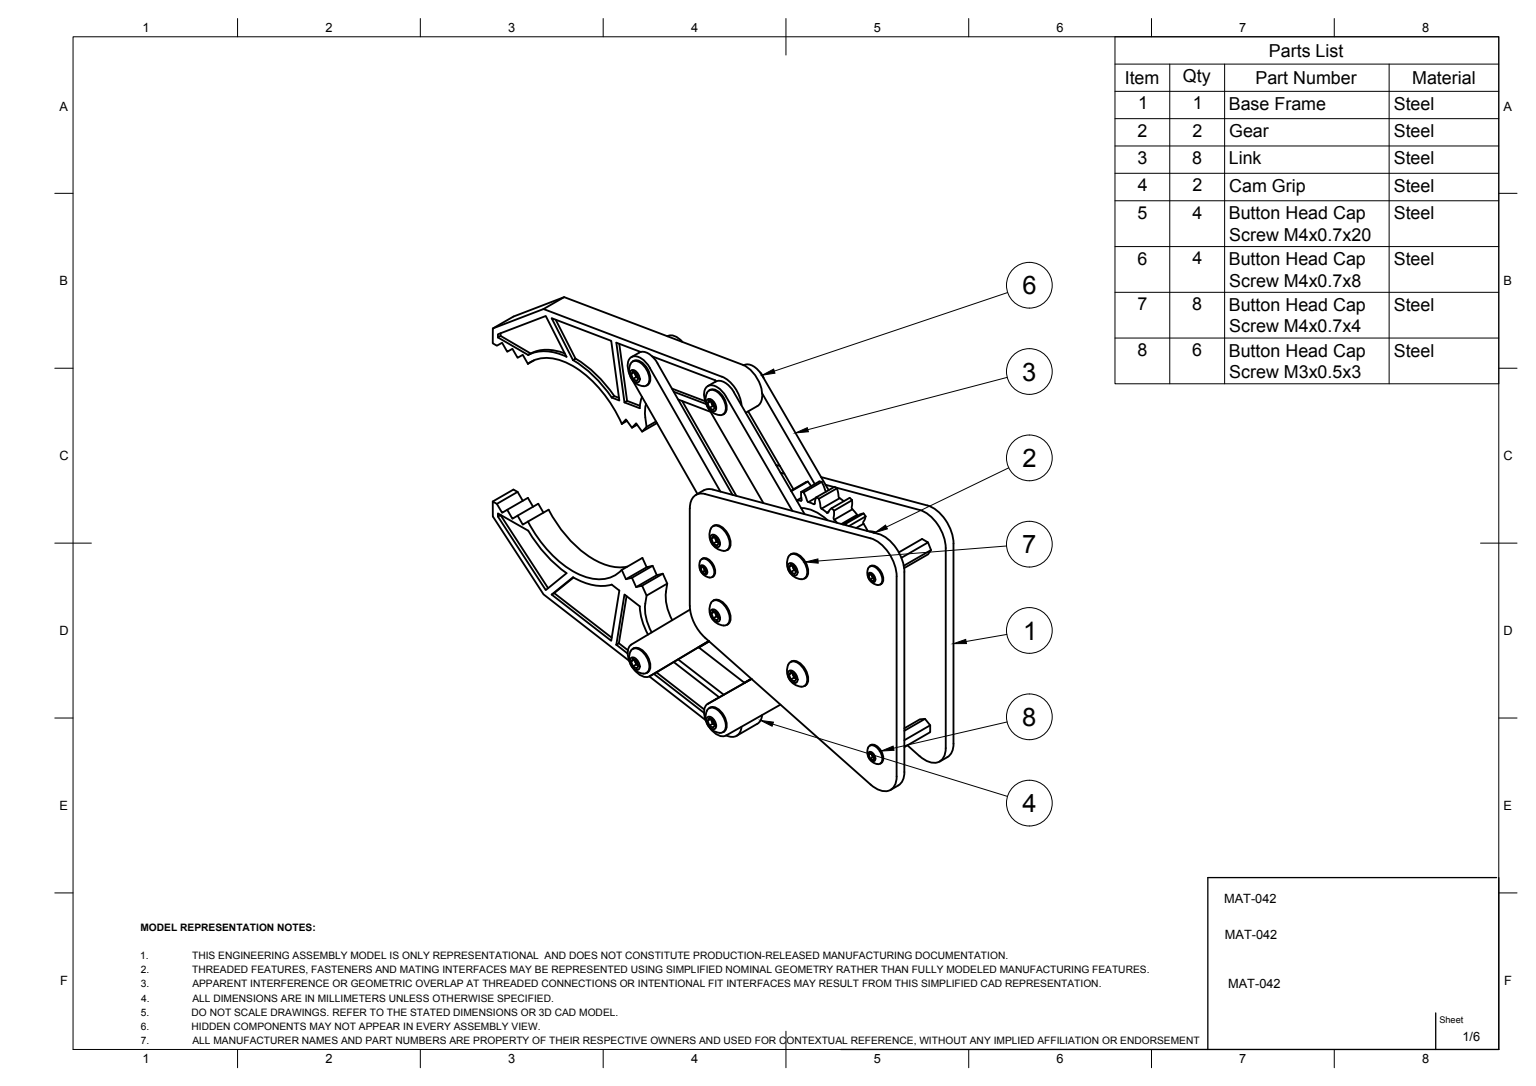
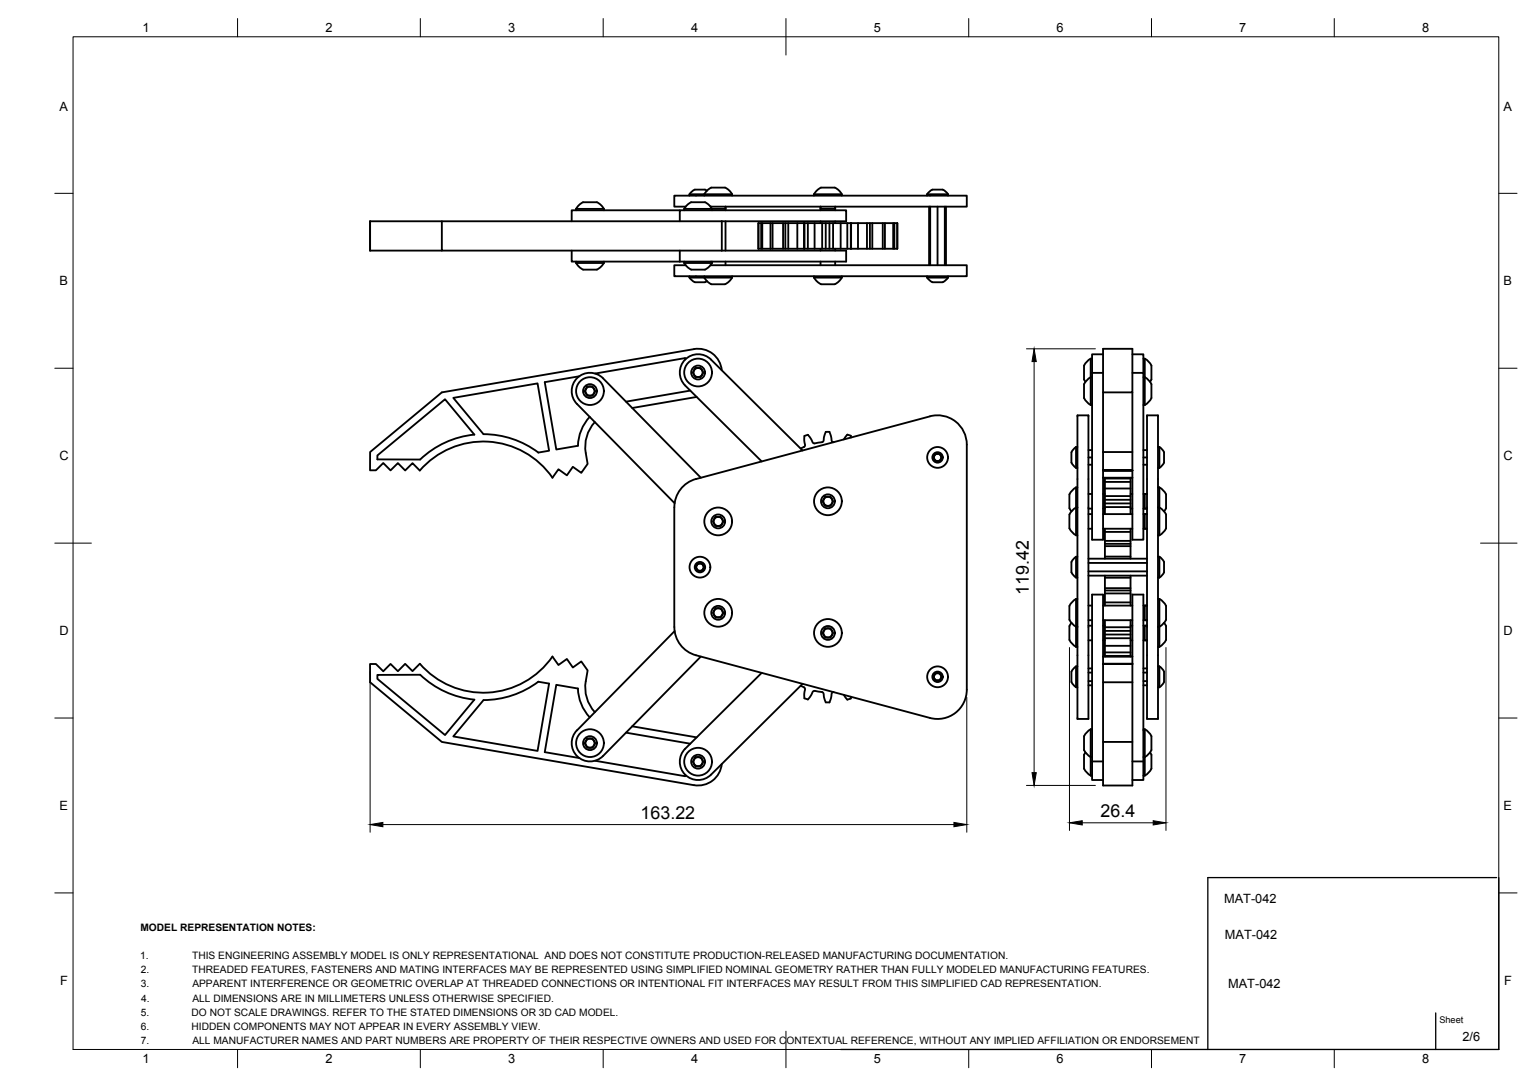
ISO-10303-21;
HEADER;
/* Generated by software containing ST-Developer
 * from STEP Tools, Inc. (www.steptools.com) 
 */

FILE_DESCRIPTION(
/* description */ ('STEP AP214'),
/* implementation_level */ '2;1');

FILE_NAME(
/* name */ 'MAT-042.step',
/* time_stamp */ '2026-11-14T22:03:06-08:00',
/* author */ (''),
/* organization */ (''),
/* preprocessor_version */ 'ST-DEVELOPER v20.2',
/* originating_system */ 'Autodesk Translation Framework v15.17.0.0',
/* authorisation */ '');

FILE_SCHEMA (('AUTOMOTIVE_DESIGN { 1 0 10303 214 3 1 1 }'));
ENDSEC;

DATA;
#10=MECHANICAL_DESIGN_GEOMETRIC_PRESENTATION_REPRESENTATION('',(#303,#304,
#305,#306,#307,#308,#309,#310,#311,#312,#313,#314),#12966);
#11=ITEM_DEFINED_TRANSFORMATION($,$,#5680,#6187);
#12=ITEM_DEFINED_TRANSFORMATION($,$,#5884,#6188);
#13=ITEM_DEFINED_TRANSFORMATION($,$,#6026,#6189);
#14=ITEM_DEFINED_TRANSFORMATION($,$,#5783,#6190);
#15=ITEM_DEFINED_TRANSFORMATION($,$,#6043,#6191);
#16=ITEM_DEFINED_TRANSFORMATION($,$,#6079,#6192);
#17=ITEM_DEFINED_TRANSFORMATION($,$,#6115,#6193);
#18=ITEM_DEFINED_TRANSFORMATION($,$,#6151,#6194);
#19=ITEM_DEFINED_TRANSFORMATION($,$,#5783,#6195);
#20=ITEM_DEFINED_TRANSFORMATION($,$,#6026,#6196);
#21=ITEM_DEFINED_TRANSFORMATION($,$,#6026,#6197);
#22=ITEM_DEFINED_TRANSFORMATION($,$,#6026,#6198);
#23=ITEM_DEFINED_TRANSFORMATION($,$,#5884,#6199);
#24=ITEM_DEFINED_TRANSFORMATION($,$,#6026,#6200);
#25=ITEM_DEFINED_TRANSFORMATION($,$,#6026,#6201);
#26=ITEM_DEFINED_TRANSFORMATION($,$,#6026,#6202);
#27=ITEM_DEFINED_TRANSFORMATION($,$,#6026,#6203);
#28=ITEM_DEFINED_TRANSFORMATION($,$,#6043,#6204);
#29=ITEM_DEFINED_TRANSFORMATION($,$,#6043,#6205);
#30=ITEM_DEFINED_TRANSFORMATION($,$,#6043,#6206);
#31=ITEM_DEFINED_TRANSFORMATION($,$,#6079,#6207);
#32=ITEM_DEFINED_TRANSFORMATION($,$,#6079,#6208);
#33=ITEM_DEFINED_TRANSFORMATION($,$,#6079,#6209);
#34=ITEM_DEFINED_TRANSFORMATION($,$,#6115,#6210);
#35=ITEM_DEFINED_TRANSFORMATION($,$,#6115,#6211);
#36=ITEM_DEFINED_TRANSFORMATION($,$,#6115,#6212);
#37=ITEM_DEFINED_TRANSFORMATION($,$,#6115,#6213);
#38=ITEM_DEFINED_TRANSFORMATION($,$,#6115,#6214);
#39=ITEM_DEFINED_TRANSFORMATION($,$,#6115,#6215);
#40=ITEM_DEFINED_TRANSFORMATION($,$,#6115,#6216);
#41=ITEM_DEFINED_TRANSFORMATION($,$,#6151,#6217);
#42=ITEM_DEFINED_TRANSFORMATION($,$,#6151,#6218);
#43=ITEM_DEFINED_TRANSFORMATION($,$,#6151,#6219);
#44=ITEM_DEFINED_TRANSFORMATION($,$,#6151,#6220);
#45=ITEM_DEFINED_TRANSFORMATION($,$,#6151,#6221);
#46=(
REPRESENTATION_RELATIONSHIP($,$,#13025,#13024)
REPRESENTATION_RELATIONSHIP_WITH_TRANSFORMATION(#11)
SHAPE_REPRESENTATION_RELATIONSHIP()
);
#47=(
REPRESENTATION_RELATIONSHIP($,$,#13027,#13024)
REPRESENTATION_RELATIONSHIP_WITH_TRANSFORMATION(#12)
SHAPE_REPRESENTATION_RELATIONSHIP()
);
#48=(
REPRESENTATION_RELATIONSHIP($,$,#13028,#13024)
REPRESENTATION_RELATIONSHIP_WITH_TRANSFORMATION(#13)
SHAPE_REPRESENTATION_RELATIONSHIP()
);
#49=(
REPRESENTATION_RELATIONSHIP($,$,#13026,#13024)
REPRESENTATION_RELATIONSHIP_WITH_TRANSFORMATION(#14)
SHAPE_REPRESENTATION_RELATIONSHIP()
);
#50=(
REPRESENTATION_RELATIONSHIP($,$,#13029,#13024)
REPRESENTATION_RELATIONSHIP_WITH_TRANSFORMATION(#15)
SHAPE_REPRESENTATION_RELATIONSHIP()
);
#51=(
REPRESENTATION_RELATIONSHIP($,$,#13030,#13024)
REPRESENTATION_RELATIONSHIP_WITH_TRANSFORMATION(#16)
SHAPE_REPRESENTATION_RELATIONSHIP()
);
#52=(
REPRESENTATION_RELATIONSHIP($,$,#13031,#13024)
REPRESENTATION_RELATIONSHIP_WITH_TRANSFORMATION(#17)
SHAPE_REPRESENTATION_RELATIONSHIP()
);
#53=(
REPRESENTATION_RELATIONSHIP($,$,#13032,#13024)
REPRESENTATION_RELATIONSHIP_WITH_TRANSFORMATION(#18)
SHAPE_REPRESENTATION_RELATIONSHIP()
);
#54=(
REPRESENTATION_RELATIONSHIP($,$,#13026,#13024)
REPRESENTATION_RELATIONSHIP_WITH_TRANSFORMATION(#19)
SHAPE_REPRESENTATION_RELATIONSHIP()
);
#55=(
REPRESENTATION_RELATIONSHIP($,$,#13028,#13024)
REPRESENTATION_RELATIONSHIP_WITH_TRANSFORMATION(#20)
SHAPE_REPRESENTATION_RELATIONSHIP()
);
#56=(
REPRESENTATION_RELATIONSHIP($,$,#13028,#13024)
REPRESENTATION_RELATIONSHIP_WITH_TRANSFORMATION(#21)
SHAPE_REPRESENTATION_RELATIONSHIP()
);
#57=(
REPRESENTATION_RELATIONSHIP($,$,#13028,#13024)
REPRESENTATION_RELATIONSHIP_WITH_TRANSFORMATION(#22)
SHAPE_REPRESENTATION_RELATIONSHIP()
);
#58=(
REPRESENTATION_RELATIONSHIP($,$,#13027,#13024)
REPRESENTATION_RELATIONSHIP_WITH_TRANSFORMATION(#23)
SHAPE_REPRESENTATION_RELATIONSHIP()
);
#59=(
REPRESENTATION_RELATIONSHIP($,$,#13028,#13024)
REPRESENTATION_RELATIONSHIP_WITH_TRANSFORMATION(#24)
SHAPE_REPRESENTATION_RELATIONSHIP()
);
#60=(
REPRESENTATION_RELATIONSHIP($,$,#13028,#13024)
REPRESENTATION_RELATIONSHIP_WITH_TRANSFORMATION(#25)
SHAPE_REPRESENTATION_RELATIONSHIP()
);
#61=(
REPRESENTATION_RELATIONSHIP($,$,#13028,#13024)
REPRESENTATION_RELATIONSHIP_WITH_TRANSFORMATION(#26)
SHAPE_REPRESENTATION_RELATIONSHIP()
);
#62=(
REPRESENTATION_RELATIONSHIP($,$,#13028,#13024)
REPRESENTATION_RELATIONSHIP_WITH_TRANSFORMATION(#27)
SHAPE_REPRESENTATION_RELATIONSHIP()
);
#63=(
REPRESENTATION_RELATIONSHIP($,$,#13029,#13024)
REPRESENTATION_RELATIONSHIP_WITH_TRANSFORMATION(#28)
SHAPE_REPRESENTATION_RELATIONSHIP()
);
#64=(
REPRESENTATION_RELATIONSHIP($,$,#13029,#13024)
REPRESENTATION_RELATIONSHIP_WITH_TRANSFORMATION(#29)
SHAPE_REPRESENTATION_RELATIONSHIP()
);
#65=(
REPRESENTATION_RELATIONSHIP($,$,#13029,#13024)
REPRESENTATION_RELATIONSHIP_WITH_TRANSFORMATION(#30)
SHAPE_REPRESENTATION_RELATIONSHIP()
);
#66=(
REPRESENTATION_RELATIONSHIP($,$,#13030,#13024)
REPRESENTATION_RELATIONSHIP_WITH_TRANSFORMATION(#31)
SHAPE_REPRESENTATION_RELATIONSHIP()
);
#67=(
REPRESENTATION_RELATIONSHIP($,$,#13030,#13024)
REPRESENTATION_RELATIONSHIP_WITH_TRANSFORMATION(#32)
SHAPE_REPRESENTATION_RELATIONSHIP()
);
#68=(
REPRESENTATION_RELATIONSHIP($,$,#13030,#13024)
REPRESENTATION_RELATIONSHIP_WITH_TRANSFORMATION(#33)
SHAPE_REPRESENTATION_RELATIONSHIP()
);
#69=(
REPRESENTATION_RELATIONSHIP($,$,#13031,#13024)
REPRESENTATION_RELATIONSHIP_WITH_TRANSFORMATION(#34)
SHAPE_REPRESENTATION_RELATIONSHIP()
);
#70=(
REPRESENTATION_RELATIONSHIP($,$,#13031,#13024)
REPRESENTATION_RELATIONSHIP_WITH_TRANSFORMATION(#35)
SHAPE_REPRESENTATION_RELATIONSHIP()
);
#71=(
REPRESENTATION_RELATIONSHIP($,$,#13031,#13024)
REPRESENTATION_RELATIONSHIP_WITH_TRANSFORMATION(#36)
SHAPE_REPRESENTATION_RELATIONSHIP()
);
#72=(
REPRESENTATION_RELATIONSHIP($,$,#13031,#13024)
REPRESENTATION_RELATIONSHIP_WITH_TRANSFORMATION(#37)
SHAPE_REPRESENTATION_RELATIONSHIP()
);
#73=(
REPRESENTATION_RELATIONSHIP($,$,#13031,#13024)
REPRESENTATION_RELATIONSHIP_WITH_TRANSFORMATION(#38)
SHAPE_REPRESENTATION_RELATIONSHIP()
);
#74=(
REPRESENTATION_RELATIONSHIP($,$,#13031,#13024)
REPRESENTATION_RELATIONSHIP_WITH_TRANSFORMATION(#39)
SHAPE_REPRESENTATION_RELATIONSHIP()
);
#75=(
REPRESENTATION_RELATIONSHIP($,$,#13031,#13024)
REPRESENTATION_RELATIONSHIP_WITH_TRANSFORMATION(#40)
SHAPE_REPRESENTATION_RELATIONSHIP()
);
#76=(
REPRESENTATION_RELATIONSHIP($,$,#13032,#13024)
REPRESENTATION_RELATIONSHIP_WITH_TRANSFORMATION(#41)
SHAPE_REPRESENTATION_RELATIONSHIP()
);
#77=(
REPRESENTATION_RELATIONSHIP($,$,#13032,#13024)
REPRESENTATION_RELATIONSHIP_WITH_TRANSFORMATION(#42)
SHAPE_REPRESENTATION_RELATIONSHIP()
);
#78=(
REPRESENTATION_RELATIONSHIP($,$,#13032,#13024)
REPRESENTATION_RELATIONSHIP_WITH_TRANSFORMATION(#43)
SHAPE_REPRESENTATION_RELATIONSHIP()
);
#79=(
REPRESENTATION_RELATIONSHIP($,$,#13032,#13024)
REPRESENTATION_RELATIONSHIP_WITH_TRANSFORMATION(#44)
SHAPE_REPRESENTATION_RELATIONSHIP()
);
#80=(
REPRESENTATION_RELATIONSHIP($,$,#13032,#13024)
REPRESENTATION_RELATIONSHIP_WITH_TRANSFORMATION(#45)
SHAPE_REPRESENTATION_RELATIONSHIP()
);
#81=CONTEXT_DEPENDENT_SHAPE_REPRESENTATION(#46,#12989);
#82=CONTEXT_DEPENDENT_SHAPE_REPRESENTATION(#47,#12990);
#83=CONTEXT_DEPENDENT_SHAPE_REPRESENTATION(#48,#12991);
#84=CONTEXT_DEPENDENT_SHAPE_REPRESENTATION(#49,#12992);
#85=CONTEXT_DEPENDENT_SHAPE_REPRESENTATION(#50,#12993);
#86=CONTEXT_DEPENDENT_SHAPE_REPRESENTATION(#51,#12994);
#87=CONTEXT_DEPENDENT_SHAPE_REPRESENTATION(#52,#12995);
#88=CONTEXT_DEPENDENT_SHAPE_REPRESENTATION(#53,#12996);
#89=CONTEXT_DEPENDENT_SHAPE_REPRESENTATION(#54,#12997);
#90=CONTEXT_DEPENDENT_SHAPE_REPRESENTATION(#55,#12998);
#91=CONTEXT_DEPENDENT_SHAPE_REPRESENTATION(#56,#12999);
#92=CONTEXT_DEPENDENT_SHAPE_REPRESENTATION(#57,#13000);
#93=CONTEXT_DEPENDENT_SHAPE_REPRESENTATION(#58,#13001);
#94=CONTEXT_DEPENDENT_SHAPE_REPRESENTATION(#59,#13002);
#95=CONTEXT_DEPENDENT_SHAPE_REPRESENTATION(#60,#13003);
#96=CONTEXT_DEPENDENT_SHAPE_REPRESENTATION(#61,#13004);
#97=CONTEXT_DEPENDENT_SHAPE_REPRESENTATION(#62,#13005);
#98=CONTEXT_DEPENDENT_SHAPE_REPRESENTATION(#63,#13006);
#99=CONTEXT_DEPENDENT_SHAPE_REPRESENTATION(#64,#13007);
#100=CONTEXT_DEPENDENT_SHAPE_REPRESENTATION(#65,#13008);
#101=CONTEXT_DEPENDENT_SHAPE_REPRESENTATION(#66,#13009);
#102=CONTEXT_DEPENDENT_SHAPE_REPRESENTATION(#67,#13010);
#103=CONTEXT_DEPENDENT_SHAPE_REPRESENTATION(#68,#13011);
#104=CONTEXT_DEPENDENT_SHAPE_REPRESENTATION(#69,#13012);
#105=CONTEXT_DEPENDENT_SHAPE_REPRESENTATION(#70,#13013);
#106=CONTEXT_DEPENDENT_SHAPE_REPRESENTATION(#71,#13014);
#107=CONTEXT_DEPENDENT_SHAPE_REPRESENTATION(#72,#13015);
#108=CONTEXT_DEPENDENT_SHAPE_REPRESENTATION(#73,#13016);
#109=CONTEXT_DEPENDENT_SHAPE_REPRESENTATION(#74,#13017);
#110=CONTEXT_DEPENDENT_SHAPE_REPRESENTATION(#75,#13018);
#111=CONTEXT_DEPENDENT_SHAPE_REPRESENTATION(#76,#13019);
#112=CONTEXT_DEPENDENT_SHAPE_REPRESENTATION(#77,#13020);
#113=CONTEXT_DEPENDENT_SHAPE_REPRESENTATION(#78,#13021);
#114=CONTEXT_DEPENDENT_SHAPE_REPRESENTATION(#79,#13022);
#115=CONTEXT_DEPENDENT_SHAPE_REPRESENTATION(#80,#13023);
#116=NEXT_ASSEMBLY_USAGE_OCCURRENCE('Base Frame:1','Base Frame:1',
'Base Frame:1',#13034,#13035,'Base Frame:1');
#117=NEXT_ASSEMBLY_USAGE_OCCURRENCE('Gear:1','Gear:1','Gear:1',#13034,#13037,
'Gear:1');
#118=NEXT_ASSEMBLY_USAGE_OCCURRENCE('Link:1','Link:1','Link:1',#13034,#13038,
'Link:1');
#119=NEXT_ASSEMBLY_USAGE_OCCURRENCE('Cam Grip:1','Cam Grip:1',
'Cam Grip:1',#13034,#13036,'Cam Grip:1');
#120=NEXT_ASSEMBLY_USAGE_OCCURRENCE('Button Head Cap Screw M4x0.7x20:1',
'Button Head Cap Screw M4x0.7x20:1','Button Head Cap Screw M4x0.7x20:1',
#13034,#13039,'Button Head Cap Screw M4x0.7x20:1');
#121=NEXT_ASSEMBLY_USAGE_OCCURRENCE('Button Head Cap Screw M4x0.7x8:1',
'Button Head Cap Screw M4x0.7x8:1','Button Head Cap Screw M4x0.7x8:1',#13034,
#13040,'Button Head Cap Screw M4x0.7x8:1');
#122=NEXT_ASSEMBLY_USAGE_OCCURRENCE('Button Head Cap Screw M4x0.7x4:1',
'Button Head Cap Screw M4x0.7x4:1','Button Head Cap Screw M4x0.7x4:1',#13034,
#13041,'Button Head Cap Screw M4x0.7x4:1');
#123=NEXT_ASSEMBLY_USAGE_OCCURRENCE('Button Head Cap Screw M3x0.5x3:1',
'Button Head Cap Screw M3x0.5x3:1','Button Head Cap Screw M3x0.5x3:1',#13034,
#13042,'Button Head Cap Screw M3x0.5x3:1');
#124=NEXT_ASSEMBLY_USAGE_OCCURRENCE('Cam Grip:2','Cam Grip:2',
'Cam Grip:2',#13034,#13036,'Cam Grip:2');
#125=NEXT_ASSEMBLY_USAGE_OCCURRENCE('Link:2','Link:2','Link:2',#13034,#13038,
'Link:2');
#126=NEXT_ASSEMBLY_USAGE_OCCURRENCE('Link:3','Link:3','Link:3',#13034,#13038,
'Link:3');
#127=NEXT_ASSEMBLY_USAGE_OCCURRENCE('Link:4','Link:4','Link:4',#13034,#13038,
'Link:4');
#128=NEXT_ASSEMBLY_USAGE_OCCURRENCE('Gear:2','Gear:2','Gear:2',#13034,#13037,
'Gear:2');
#129=NEXT_ASSEMBLY_USAGE_OCCURRENCE('Link:5','Link:5','Link:5',#13034,#13038,
'Link:5');
#130=NEXT_ASSEMBLY_USAGE_OCCURRENCE('Link:6','Link:6','Link:6',#13034,#13038,
'Link:6');
#131=NEXT_ASSEMBLY_USAGE_OCCURRENCE('Link:7','Link:7','Link:7',#13034,#13038,
'Link:7');
#132=NEXT_ASSEMBLY_USAGE_OCCURRENCE('Link:8','Link:8','Link:8',#13034,#13038,
'Link:8');
#133=NEXT_ASSEMBLY_USAGE_OCCURRENCE('Button Head Cap Screw M4x0.7x20:2',
'Button Head Cap Screw M4x0.7x20:2','Button Head Cap Screw M4x0.7x20:2',
#13034,#13039,'Button Head Cap Screw M4x0.7x20:2');
#134=NEXT_ASSEMBLY_USAGE_OCCURRENCE('Button Head Cap Screw M4x0.7x20:3',
'Button Head Cap Screw M4x0.7x20:3','Button Head Cap Screw M4x0.7x20:3',
#13034,#13039,'Button Head Cap Screw M4x0.7x20:3');
#135=NEXT_ASSEMBLY_USAGE_OCCURRENCE('Button Head Cap Screw M4x0.7x20:4',
'Button Head Cap Screw M4x0.7x20:4','Button Head Cap Screw M4x0.7x20:4',
#13034,#13039,'Button Head Cap Screw M4x0.7x20:4');
#136=NEXT_ASSEMBLY_USAGE_OCCURRENCE('Button Head Cap Screw M4x0.7x8:2',
'Button Head Cap Screw M4x0.7x8:2','Button Head Cap Screw M4x0.7x8:2',#13034,
#13040,'Button Head Cap Screw M4x0.7x8:2');
#137=NEXT_ASSEMBLY_USAGE_OCCURRENCE('Button Head Cap Screw M4x0.7x8:3',
'Button Head Cap Screw M4x0.7x8:3','Button Head Cap Screw M4x0.7x8:3',#13034,
#13040,'Button Head Cap Screw M4x0.7x8:3');
#138=NEXT_ASSEMBLY_USAGE_OCCURRENCE('Button Head Cap Screw M4x0.7x8:4',
'Button Head Cap Screw M4x0.7x8:4','Button Head Cap Screw M4x0.7x8:4',#13034,
#13040,'Button Head Cap Screw M4x0.7x8:4');
#139=NEXT_ASSEMBLY_USAGE_OCCURRENCE('Button Head Cap Screw M4x0.7x4:2',
'Button Head Cap Screw M4x0.7x4:2','Button Head Cap Screw M4x0.7x4:2',#13034,
#13041,'Button Head Cap Screw M4x0.7x4:2');
#140=NEXT_ASSEMBLY_USAGE_OCCURRENCE('Button Head Cap Screw M4x0.7x4:3',
'Button Head Cap Screw M4x0.7x4:3','Button Head Cap Screw M4x0.7x4:3',#13034,
#13041,'Button Head Cap Screw M4x0.7x4:3');
#141=NEXT_ASSEMBLY_USAGE_OCCURRENCE('Button Head Cap Screw M4x0.7x4:4',
'Button Head Cap Screw M4x0.7x4:4','Button Head Cap Screw M4x0.7x4:4',#13034,
#13041,'Button Head Cap Screw M4x0.7x4:4');
#142=NEXT_ASSEMBLY_USAGE_OCCURRENCE('Button Head Cap Screw M4x0.7x4:5',
'Button Head Cap Screw M4x0.7x4:5','Button Head Cap Screw M4x0.7x4:5',#13034,
#13041,'Button Head Cap Screw M4x0.7x4:5');
#143=NEXT_ASSEMBLY_USAGE_OCCURRENCE('Button Head Cap Screw M4x0.7x4:6',
'Button Head Cap Screw M4x0.7x4:6','Button Head Cap Screw M4x0.7x4:6',#13034,
#13041,'Button Head Cap Screw M4x0.7x4:6');
#144=NEXT_ASSEMBLY_USAGE_OCCURRENCE('Button Head Cap Screw M4x0.7x4:7',
'Button Head Cap Screw M4x0.7x4:7','Button Head Cap Screw M4x0.7x4:7',#13034,
#13041,'Button Head Cap Screw M4x0.7x4:7');
#145=NEXT_ASSEMBLY_USAGE_OCCURRENCE('Button Head Cap Screw M4x0.7x4:8',
'Button Head Cap Screw M4x0.7x4:8','Button Head Cap Screw M4x0.7x4:8',#13034,
#13041,'Button Head Cap Screw M4x0.7x4:8');
#146=NEXT_ASSEMBLY_USAGE_OCCURRENCE('Button Head Cap Screw M3x0.5x3:2',
'Button Head Cap Screw M3x0.5x3:2','Button Head Cap Screw M3x0.5x3:2',#13034,
#13042,'Button Head Cap Screw M3x0.5x3:2');
#147=NEXT_ASSEMBLY_USAGE_OCCURRENCE('Button Head Cap Screw M3x0.5x3:3',
'Button Head Cap Screw M3x0.5x3:3','Button Head Cap Screw M3x0.5x3:3',#13034,
#13042,'Button Head Cap Screw M3x0.5x3:3');
#148=NEXT_ASSEMBLY_USAGE_OCCURRENCE('Button Head Cap Screw M3x0.5x3:4',
'Button Head Cap Screw M3x0.5x3:4','Button Head Cap Screw M3x0.5x3:4',#13034,
#13042,'Button Head Cap Screw M3x0.5x3:4');
#149=NEXT_ASSEMBLY_USAGE_OCCURRENCE('Button Head Cap Screw M3x0.5x3:5',
'Button Head Cap Screw M3x0.5x3:5','Button Head Cap Screw M3x0.5x3:5',#13034,
#13042,'Button Head Cap Screw M3x0.5x3:5');
#150=NEXT_ASSEMBLY_USAGE_OCCURRENCE('Button Head Cap Screw M3x0.5x3:6',
'Button Head Cap Screw M3x0.5x3:6','Button Head Cap Screw M3x0.5x3:6',#13034,
#13042,'Button Head Cap Screw M3x0.5x3:6');
#151=SPHERICAL_SURFACE('',#6062,4.3249693283142);
#152=SPHERICAL_SURFACE('',#6098,4.3249693283142);
#153=SPHERICAL_SURFACE('',#6134,4.3249693283142);
#154=SPHERICAL_SURFACE('',#6170,3.35141684393879);
#155=TOROIDAL_SURFACE('',#6051,2.2,0.2);
#156=TOROIDAL_SURFACE('',#6087,2.2,0.2);
#157=TOROIDAL_SURFACE('',#6123,2.2,0.2);
#158=TOROIDAL_SURFACE('',#6159,1.6,0.1);
#159=CONICAL_SURFACE('',#6044,1732.05080756886,1.04719755119659);
#160=CONICAL_SURFACE('',#6055,1.61,0.785398163397453);
#161=CONICAL_SURFACE('',#6080,1732.05080756886,1.04719755119659);
#162=CONICAL_SURFACE('',#6091,1.61,0.785398163397447);
#163=CONICAL_SURFACE('',#6116,1732.05080756886,1.04719755119659);
#164=CONICAL_SURFACE('',#6127,1.61,0.785398163397447);
#165=CONICAL_SURFACE('',#6152,1732.05080756886,1.04719755119659);
#166=CONICAL_SURFACE('',#6163,1.2195,0.785398163397446);
#167=B_SPLINE_SURFACE_WITH_KNOTS('',3,1,((#10554,#10555),(#10556,#10557),
(#10558,#10559),(#10560,#10561),(#10562,#10563),(#10564,#10565),(#10566,
#10567),(#10568,#10569),(#10570,#10571),(#10572,#10573),(#10574,#10575),
(#10576,#10577),(#10578,#10579),(#10580,#10581),(#10582,#10583),(#10584,
#10585),(#10586,#10587),(#10588,#10589),(#10590,#10591),(#10592,#10593),
(#10594,#10595),(#10596,#10597),(#10598,#10599)),.UNSPECIFIED.,.F.,.F.,
 .F.,(4,1,1,1,1,1,1,1,1,1,1,1,1,1,1,1,1,1,1,1,4),(2,2),(0.0323453817713401,
0.0983189520624214,0.14064060480402,0.176193019733645,0.208307484243854,
0.23948443235858,0.271287112904486,0.28220667781497,0.293329328714142,0.304676551002397,
0.319437818234531,0.350137192454192,0.38765864687273,0.432002181900136,
0.483167797782405,0.541155494678712,0.605965272697963,0.67759713191795,
0.75605107239617,0.841327094176323,1.),(0.,0.84),.UNSPECIFIED.);
#168=B_SPLINE_SURFACE_WITH_KNOTS('',3,1,((#10604,#10605),(#10606,#10607),
(#10608,#10609),(#10610,#10611),(#10612,#10613),(#10614,#10615),(#10616,
#10617),(#10618,#10619),(#10620,#10621),(#10622,#10623),(#10624,#10625),
(#10626,#10627),(#10628,#10629),(#10630,#10631),(#10632,#10633),(#10634,
#10635),(#10636,#10637),(#10638,#10639),(#10640,#10641),(#10642,#10643),
(#10644,#10645),(#10646,#10647),(#10648,#10649)),.UNSPECIFIED.,.F.,.F.,
 .F.,(4,1,1,1,1,1,1,1,1,1,1,1,1,1,1,1,1,1,1,1,4),(2,2),(0.,0.158672905823676,
0.243948927603829,0.322402868082049,0.394034727302036,0.458844505321287,
0.516832202217594,0.567997818099863,0.612341353127269,0.649862807545807,
0.680562181765468,0.695323448997602,0.706670671285856,0.717793322185029,
0.728712887095513,0.760515567641419,0.791692515756145,0.823806980266354,
0.859359395195979,0.901681047937578,0.967654618228659),(0.,0.839999999999999),
 .UNSPECIFIED.);
#169=B_SPLINE_SURFACE_WITH_KNOTS('',3,1,((#10653,#10654),(#10655,#10656),
(#10657,#10658),(#10659,#10660),(#10661,#10662),(#10663,#10664),(#10665,
#10666),(#10667,#10668),(#10669,#10670),(#10671,#10672),(#10673,#10674),
(#10675,#10676),(#10677,#10678),(#10679,#10680),(#10681,#10682),(#10683,
#10684),(#10685,#10686),(#10687,#10688),(#10689,#10690),(#10691,#10692),
(#10693,#10694),(#10695,#10696),(#10697,#10698)),.UNSPECIFIED.,.F.,.F.,
 .F.,(4,1,1,1,1,1,1,1,1,1,1,1,1,1,1,1,1,1,1,1,4),(2,2),(0.0323453817713401,
0.0983189520624214,0.14064060480402,0.176193019733645,0.208307484243854,
0.23948443235858,0.271287112904486,0.28220667781497,0.293329328714142,0.304676551002397,
0.319437818234531,0.350137192454192,0.38765864687273,0.432002181900136,
0.483167797782405,0.541155494678712,0.605965272697963,0.67759713191795,
0.75605107239617,0.841327094176323,1.),(0.,0.84),.UNSPECIFIED.);
#170=B_SPLINE_SURFACE_WITH_KNOTS('',3,1,((#10702,#10703),(#10704,#10705),
(#10706,#10707),(#10708,#10709),(#10710,#10711),(#10712,#10713),(#10714,
#10715),(#10716,#10717),(#10718,#10719),(#10720,#10721),(#10722,#10723),
(#10724,#10725),(#10726,#10727),(#10728,#10729),(#10730,#10731),(#10732,
#10733),(#10734,#10735),(#10736,#10737),(#10738,#10739),(#10740,#10741),
(#10742,#10743),(#10744,#10745),(#10746,#10747)),.UNSPECIFIED.,.F.,.F.,
 .F.,(4,1,1,1,1,1,1,1,1,1,1,1,1,1,1,1,1,1,1,1,4),(2,2),(0.,0.158672905823676,
0.243948927603829,0.322402868082049,0.394034727302036,0.458844505321287,
0.516832202217594,0.567997818099863,0.612341353127269,0.649862807545807,
0.680562181765468,0.695323448997602,0.706670671285856,0.717793322185029,
0.728712887095513,0.760515567641419,0.791692515756145,0.823806980266354,
0.859359395195979,0.901681047937578,0.967654618228659),(0.,0.839999999999998),
 .UNSPECIFIED.);
#171=B_SPLINE_SURFACE_WITH_KNOTS('',3,1,((#10751,#10752),(#10753,#10754),
(#10755,#10756),(#10757,#10758),(#10759,#10760),(#10761,#10762),(#10763,
#10764),(#10765,#10766),(#10767,#10768),(#10769,#10770),(#10771,#10772),
(#10773,#10774),(#10775,#10776),(#10777,#10778),(#10779,#10780),(#10781,
#10782),(#10783,#10784),(#10785,#10786),(#10787,#10788),(#10789,#10790),
(#10791,#10792),(#10793,#10794),(#10795,#10796)),.UNSPECIFIED.,.F.,.F.,
 .F.,(4,1,1,1,1,1,1,1,1,1,1,1,1,1,1,1,1,1,1,1,4),(2,2),(0.0323453817713401,
0.0983189520624214,0.14064060480402,0.176193019733645,0.208307484243854,
0.23948443235858,0.271287112904486,0.28220667781497,0.293329328714142,0.304676551002397,
0.319437818234531,0.350137192454192,0.38765864687273,0.432002181900136,
0.483167797782405,0.541155494678712,0.605965272697963,0.67759713191795,
0.75605107239617,0.841327094176323,1.),(0.,0.84),.UNSPECIFIED.);
#172=B_SPLINE_SURFACE_WITH_KNOTS('',3,1,((#10800,#10801),(#10802,#10803),
(#10804,#10805),(#10806,#10807),(#10808,#10809),(#10810,#10811),(#10812,
#10813),(#10814,#10815),(#10816,#10817),(#10818,#10819),(#10820,#10821),
(#10822,#10823),(#10824,#10825),(#10826,#10827),(#10828,#10829),(#10830,
#10831),(#10832,#10833),(#10834,#10835),(#10836,#10837),(#10838,#10839),
(#10840,#10841),(#10842,#10843),(#10844,#10845)),.UNSPECIFIED.,.F.,.F.,
 .F.,(4,1,1,1,1,1,1,1,1,1,1,1,1,1,1,1,1,1,1,1,4),(2,2),(0.,0.158672905823676,
0.243948927603829,0.322402868082049,0.394034727302036,0.458844505321287,
0.516832202217594,0.567997818099863,0.612341353127269,0.649862807545807,
0.680562181765468,0.695323448997602,0.706670671285856,0.717793322185029,
0.728712887095513,0.760515567641419,0.791692515756145,0.823806980266354,
0.859359395195979,0.901681047937578,0.967654618228659),(0.,0.839999999999999),
 .UNSPECIFIED.);
#173=B_SPLINE_SURFACE_WITH_KNOTS('',3,1,((#10849,#10850),(#10851,#10852),
(#10853,#10854),(#10855,#10856),(#10857,#10858),(#10859,#10860),(#10861,
#10862),(#10863,#10864),(#10865,#10866),(#10867,#10868),(#10869,#10870),
(#10871,#10872),(#10873,#10874),(#10875,#10876),(#10877,#10878),(#10879,
#10880),(#10881,#10882),(#10883,#10884),(#10885,#10886),(#10887,#10888),
(#10889,#10890),(#10891,#10892),(#10893,#10894)),.UNSPECIFIED.,.F.,.F.,
 .F.,(4,1,1,1,1,1,1,1,1,1,1,1,1,1,1,1,1,1,1,1,4),(2,2),(0.0323453817713401,
0.0983189520624214,0.14064060480402,0.176193019733645,0.208307484243854,
0.23948443235858,0.271287112904486,0.28220667781497,0.293329328714142,0.304676551002397,
0.319437818234531,0.350137192454192,0.38765864687273,0.432002181900136,
0.483167797782405,0.541155494678712,0.605965272697963,0.67759713191795,
0.75605107239617,0.841327094176323,1.),(0.,0.840000000000002),
 .UNSPECIFIED.);
#174=B_SPLINE_SURFACE_WITH_KNOTS('',3,1,((#10898,#10899),(#10900,#10901),
(#10902,#10903),(#10904,#10905),(#10906,#10907),(#10908,#10909),(#10910,
#10911),(#10912,#10913),(#10914,#10915),(#10916,#10917),(#10918,#10919),
(#10920,#10921),(#10922,#10923),(#10924,#10925),(#10926,#10927),(#10928,
#10929),(#10930,#10931),(#10932,#10933),(#10934,#10935),(#10936,#10937),
(#10938,#10939),(#10940,#10941),(#10942,#10943)),.UNSPECIFIED.,.F.,.F.,
 .F.,(4,1,1,1,1,1,1,1,1,1,1,1,1,1,1,1,1,1,1,1,4),(2,2),(0.,0.158672905823676,
0.243948927603829,0.322402868082049,0.394034727302036,0.458844505321287,
0.516832202217594,0.567997818099863,0.612341353127269,0.649862807545807,
0.680562181765468,0.695323448997602,0.706670671285856,0.717793322185029,
0.728712887095513,0.760515567641419,0.791692515756145,0.823806980266354,
0.859359395195979,0.901681047937578,0.967654618228659),(0.,0.84),
 .UNSPECIFIED.);
#175=B_SPLINE_SURFACE_WITH_KNOTS('',3,1,((#10947,#10948),(#10949,#10950),
(#10951,#10952),(#10953,#10954),(#10955,#10956),(#10957,#10958),(#10959,
#10960),(#10961,#10962),(#10963,#10964),(#10965,#10966),(#10967,#10968),
(#10969,#10970),(#10971,#10972),(#10973,#10974),(#10975,#10976),(#10977,
#10978),(#10979,#10980),(#10981,#10982),(#10983,#10984),(#10985,#10986),
(#10987,#10988),(#10989,#10990),(#10991,#10992)),.UNSPECIFIED.,.F.,.F.,
 .F.,(4,1,1,1,1,1,1,1,1,1,1,1,1,1,1,1,1,1,1,1,4),(2,2),(0.0323453817713401,
0.0983189520624214,0.14064060480402,0.176193019733645,0.208307484243854,
0.23948443235858,0.271287112904486,0.28220667781497,0.293329328714142,0.304676551002397,
0.319437818234531,0.350137192454192,0.38765864687273,0.432002181900136,
0.483167797782405,0.541155494678712,0.605965272697963,0.67759713191795,
0.75605107239617,0.841327094176323,1.),(0.,0.84),.UNSPECIFIED.);
#176=B_SPLINE_SURFACE_WITH_KNOTS('',3,1,((#10996,#10997),(#10998,#10999),
(#11000,#11001),(#11002,#11003),(#11004,#11005),(#11006,#11007),(#11008,
#11009),(#11010,#11011),(#11012,#11013),(#11014,#11015),(#11016,#11017),
(#11018,#11019),(#11020,#11021),(#11022,#11023),(#11024,#11025),(#11026,
#11027),(#11028,#11029),(#11030,#11031),(#11032,#11033),(#11034,#11035),
(#11036,#11037),(#11038,#11039),(#11040,#11041)),.UNSPECIFIED.,.F.,.F.,
 .F.,(4,1,1,1,1,1,1,1,1,1,1,1,1,1,1,1,1,1,1,1,4),(2,2),(0.,0.158672905823676,
0.243948927603829,0.322402868082049,0.394034727302036,0.458844505321287,
0.516832202217594,0.567997818099863,0.612341353127269,0.649862807545807,
0.680562181765468,0.695323448997602,0.706670671285856,0.717793322185029,
0.728712887095513,0.760515567641419,0.791692515756145,0.823806980266354,
0.859359395195979,0.901681047937578,0.967654618228659),(0.,0.839999999999999),
 .UNSPECIFIED.);
#177=B_SPLINE_SURFACE_WITH_KNOTS('',3,1,((#11045,#11046),(#11047,#11048),
(#11049,#11050),(#11051,#11052),(#11053,#11054),(#11055,#11056),(#11057,
#11058),(#11059,#11060),(#11061,#11062),(#11063,#11064),(#11065,#11066),
(#11067,#11068),(#11069,#11070),(#11071,#11072),(#11073,#11074),(#11075,
#11076),(#11077,#11078),(#11079,#11080),(#11081,#11082),(#11083,#11084),
(#11085,#11086),(#11087,#11088),(#11089,#11090)),.UNSPECIFIED.,.F.,.F.,
 .F.,(4,1,1,1,1,1,1,1,1,1,1,1,1,1,1,1,1,1,1,1,4),(2,2),(0.0323453817713401,
0.0983189520624214,0.14064060480402,0.176193019733645,0.208307484243854,
0.23948443235858,0.271287112904486,0.28220667781497,0.293329328714142,0.304676551002397,
0.319437818234531,0.350137192454192,0.38765864687273,0.432002181900136,
0.483167797782405,0.541155494678712,0.605965272697963,0.67759713191795,
0.75605107239617,0.841327094176323,1.),(0.,0.84),.UNSPECIFIED.);
#178=B_SPLINE_SURFACE_WITH_KNOTS('',3,1,((#11094,#11095),(#11096,#11097),
(#11098,#11099),(#11100,#11101),(#11102,#11103),(#11104,#11105),(#11106,
#11107),(#11108,#11109),(#11110,#11111),(#11112,#11113),(#11114,#11115),
(#11116,#11117),(#11118,#11119),(#11120,#11121),(#11122,#11123),(#11124,
#11125),(#11126,#11127),(#11128,#11129),(#11130,#11131),(#11132,#11133),
(#11134,#11135),(#11136,#11137),(#11138,#11139)),.UNSPECIFIED.,.F.,.F.,
 .F.,(4,1,1,1,1,1,1,1,1,1,1,1,1,1,1,1,1,1,1,1,4),(2,2),(0.,0.158672905823676,
0.243948927603829,0.322402868082049,0.394034727302036,0.458844505321287,
0.516832202217594,0.567997818099863,0.612341353127269,0.649862807545807,
0.680562181765468,0.695323448997602,0.706670671285856,0.717793322185029,
0.728712887095513,0.760515567641419,0.791692515756145,0.823806980266354,
0.859359395195979,0.901681047937578,0.967654618228659),(0.,0.84),
 .UNSPECIFIED.);
#179=B_SPLINE_SURFACE_WITH_KNOTS('',3,1,((#11143,#11144),(#11145,#11146),
(#11147,#11148),(#11149,#11150),(#11151,#11152),(#11153,#11154),(#11155,
#11156),(#11157,#11158),(#11159,#11160),(#11161,#11162),(#11163,#11164),
(#11165,#11166),(#11167,#11168),(#11169,#11170),(#11171,#11172),(#11173,
#11174),(#11175,#11176),(#11177,#11178),(#11179,#11180),(#11181,#11182),
(#11183,#11184),(#11185,#11186),(#11187,#11188)),.UNSPECIFIED.,.F.,.F.,
 .F.,(4,1,1,1,1,1,1,1,1,1,1,1,1,1,1,1,1,1,1,1,4),(2,2),(0.0323453817713401,
0.0983189520624214,0.14064060480402,0.176193019733645,0.208307484243854,
0.23948443235858,0.271287112904486,0.28220667781497,0.293329328714142,0.304676551002397,
0.319437818234531,0.350137192454192,0.38765864687273,0.432002181900136,
0.483167797782405,0.541155494678712,0.605965272697963,0.67759713191795,
0.75605107239617,0.841327094176323,1.),(0.,0.84),.UNSPECIFIED.);
#180=B_SPLINE_SURFACE_WITH_KNOTS('',3,1,((#11192,#11193),(#11194,#11195),
(#11196,#11197),(#11198,#11199),(#11200,#11201),(#11202,#11203),(#11204,
#11205),(#11206,#11207),(#11208,#11209),(#11210,#11211),(#11212,#11213),
(#11214,#11215),(#11216,#11217),(#11218,#11219),(#11220,#11221),(#11222,
#11223),(#11224,#11225),(#11226,#11227),(#11228,#11229),(#11230,#11231),
(#11232,#11233),(#11234,#11235),(#11236,#11237)),.UNSPECIFIED.,.F.,.F.,
 .F.,(4,1,1,1,1,1,1,1,1,1,1,1,1,1,1,1,1,1,1,1,4),(2,2),(0.,0.158672905823676,
0.243948927603829,0.322402868082049,0.394034727302036,0.458844505321287,
0.516832202217594,0.567997818099863,0.612341353127269,0.649862807545807,
0.680562181765468,0.695323448997602,0.706670671285856,0.717793322185029,
0.728712887095513,0.760515567641419,0.791692515756145,0.823806980266354,
0.859359395195979,0.901681047937578,0.967654618228659),(0.,0.84),
 .UNSPECIFIED.);
#181=B_SPLINE_SURFACE_WITH_KNOTS('',3,1,((#11241,#11242),(#11243,#11244),
(#11245,#11246),(#11247,#11248),(#11249,#11250),(#11251,#11252),(#11253,
#11254),(#11255,#11256),(#11257,#11258),(#11259,#11260),(#11261,#11262),
(#11263,#11264),(#11265,#11266),(#11267,#11268),(#11269,#11270),(#11271,
#11272),(#11273,#11274),(#11275,#11276),(#11277,#11278),(#11279,#11280),
(#11281,#11282),(#11283,#11284),(#11285,#11286)),.UNSPECIFIED.,.F.,.F.,
 .F.,(4,1,1,1,1,1,1,1,1,1,1,1,1,1,1,1,1,1,1,1,4),(2,2),(0.0323453817713401,
0.0983189520624214,0.14064060480402,0.176193019733645,0.208307484243854,
0.23948443235858,0.271287112904486,0.28220667781497,0.293329328714142,0.304676551002397,
0.319437818234531,0.350137192454192,0.38765864687273,0.432002181900136,
0.483167797782405,0.541155494678712,0.605965272697963,0.67759713191795,
0.75605107239617,0.841327094176323,1.),(0.,0.84),.UNSPECIFIED.);
#182=B_SPLINE_SURFACE_WITH_KNOTS('',3,1,((#11290,#11291),(#11292,#11293),
(#11294,#11295),(#11296,#11297),(#11298,#11299),(#11300,#11301),(#11302,
#11303),(#11304,#11305),(#11306,#11307),(#11308,#11309),(#11310,#11311),
(#11312,#11313),(#11314,#11315),(#11316,#11317),(#11318,#11319),(#11320,
#11321),(#11322,#11323),(#11324,#11325),(#11326,#11327),(#11328,#11329),
(#11330,#11331),(#11332,#11333),(#11334,#11335)),.UNSPECIFIED.,.F.,.F.,
 .F.,(4,1,1,1,1,1,1,1,1,1,1,1,1,1,1,1,1,1,1,1,4),(2,2),(0.,0.158672905823676,
0.243948927603829,0.322402868082049,0.394034727302036,0.458844505321287,
0.516832202217594,0.567997818099863,0.612341353127269,0.649862807545807,
0.680562181765468,0.695323448997602,0.706670671285856,0.717793322185029,
0.728712887095513,0.760515567641419,0.791692515756145,0.823806980266354,
0.859359395195979,0.901681047937578,0.967654618228659),(0.,0.839999999999999),
 .UNSPECIFIED.);
#183=B_SPLINE_SURFACE_WITH_KNOTS('',3,1,((#11339,#11340),(#11341,#11342),
(#11343,#11344),(#11345,#11346),(#11347,#11348),(#11349,#11350),(#11351,
#11352),(#11353,#11354),(#11355,#11356),(#11357,#11358),(#11359,#11360),
(#11361,#11362),(#11363,#11364),(#11365,#11366),(#11367,#11368),(#11369,
#11370),(#11371,#11372),(#11373,#11374),(#11375,#11376),(#11377,#11378),
(#11379,#11380),(#11381,#11382),(#11383,#11384)),.UNSPECIFIED.,.F.,.F.,
 .F.,(4,1,1,1,1,1,1,1,1,1,1,1,1,1,1,1,1,1,1,1,4),(2,2),(0.0323453817713401,
0.0983189520624214,0.14064060480402,0.176193019733645,0.208307484243854,
0.23948443235858,0.271287112904486,0.28220667781497,0.293329328714142,0.304676551002397,
0.319437818234531,0.350137192454192,0.38765864687273,0.432002181900136,
0.483167797782405,0.541155494678712,0.605965272697963,0.67759713191795,
0.75605107239617,0.841327094176323,1.),(0.,0.84),.UNSPECIFIED.);
#184=B_SPLINE_SURFACE_WITH_KNOTS('',3,1,((#11388,#11389),(#11390,#11391),
(#11392,#11393),(#11394,#11395),(#11396,#11397),(#11398,#11399),(#11400,
#11401),(#11402,#11403),(#11404,#11405),(#11406,#11407),(#11408,#11409),
(#11410,#11411),(#11412,#11413),(#11414,#11415),(#11416,#11417),(#11418,
#11419),(#11420,#11421),(#11422,#11423),(#11424,#11425),(#11426,#11427),
(#11428,#11429),(#11430,#11431),(#11432,#11433)),.UNSPECIFIED.,.F.,.F.,
 .F.,(4,1,1,1,1,1,1,1,1,1,1,1,1,1,1,1,1,1,1,1,4),(2,2),(0.,0.158672905823676,
0.243948927603829,0.322402868082049,0.394034727302036,0.458844505321287,
0.516832202217594,0.567997818099863,0.612341353127269,0.649862807545807,
0.680562181765468,0.695323448997602,0.706670671285856,0.717793322185029,
0.728712887095513,0.760515567641419,0.791692515756145,0.823806980266354,
0.859359395195979,0.901681047937578,0.967654618228659),(0.,0.839999999999999),
 .UNSPECIFIED.);
#185=B_SPLINE_SURFACE_WITH_KNOTS('',3,1,((#11434,#11435),(#11436,#11437),
(#11438,#11439),(#11440,#11441),(#11442,#11443),(#11444,#11445),(#11446,
#11447),(#11448,#11449),(#11450,#11451),(#11452,#11453),(#11454,#11455),
(#11456,#11457),(#11458,#11459),(#11460,#11461),(#11462,#11463),(#11464,
#11465),(#11466,#11467),(#11468,#11469),(#11470,#11471),(#11472,#11473),
(#11474,#11475),(#11476,#11477),(#11478,#11479)),.UNSPECIFIED.,.F.,.F.,
 .F.,(4,1,1,1,1,1,1,1,1,1,1,1,1,1,1,1,1,1,1,1,4),(2,2),(0.0323453817713401,
0.0983189520624214,0.14064060480402,0.176193019733645,0.208307484243854,
0.23948443235858,0.271287112904486,0.28220667781497,0.293329328714142,0.304676551002397,
0.319437818234531,0.350137192454192,0.38765864687273,0.432002181900136,
0.483167797782405,0.541155494678712,0.605965272697963,0.67759713191795,
0.75605107239617,0.841327094176323,1.),(0.,0.84),.UNSPECIFIED.);
#186=B_SPLINE_SURFACE_WITH_KNOTS('',3,1,((#11483,#11484),(#11485,#11486),
(#11487,#11488),(#11489,#11490),(#11491,#11492),(#11493,#11494),(#11495,
#11496),(#11497,#11498),(#11499,#11500),(#11501,#11502),(#11503,#11504),
(#11505,#11506),(#11507,#11508),(#11509,#11510),(#11511,#11512),(#11513,
#11514),(#11515,#11516),(#11517,#11518),(#11519,#11520),(#11521,#11522),
(#11523,#11524),(#11525,#11526),(#11527,#11528)),.UNSPECIFIED.,.F.,.F.,
 .F.,(4,1,1,1,1,1,1,1,1,1,1,1,1,1,1,1,1,1,1,1,4),(2,2),(0.,0.158672905823676,
0.243948927603829,0.322402868082049,0.394034727302036,0.458844505321287,
0.516832202217594,0.567997818099863,0.612341353127269,0.649862807545807,
0.680562181765468,0.695323448997602,0.706670671285856,0.717793322185029,
0.728712887095513,0.760515567641419,0.791692515756145,0.823806980266354,
0.859359395195979,0.901681047937578,0.967654618228659),(0.,0.839999999999999),
 .UNSPECIFIED.);
#187=B_SPLINE_SURFACE_WITH_KNOTS('',3,1,((#11532,#11533),(#11534,#11535),
(#11536,#11537),(#11538,#11539),(#11540,#11541),(#11542,#11543),(#11544,
#11545),(#11546,#11547),(#11548,#11549),(#11550,#11551),(#11552,#11553),
(#11554,#11555),(#11556,#11557),(#11558,#11559),(#11560,#11561),(#11562,
#11563),(#11564,#11565),(#11566,#11567),(#11568,#11569),(#11570,#11571),
(#11572,#11573),(#11574,#11575),(#11576,#11577)),.UNSPECIFIED.,.F.,.F.,
 .F.,(4,1,1,1,1,1,1,1,1,1,1,1,1,1,1,1,1,1,1,1,4),(2,2),(0.0323453817713401,
0.0983189520624214,0.14064060480402,0.176193019733645,0.208307484243854,
0.23948443235858,0.271287112904486,0.28220667781497,0.293329328714142,0.304676551002397,
0.319437818234531,0.350137192454192,0.38765864687273,0.432002181900136,
0.483167797782405,0.541155494678712,0.605965272697963,0.67759713191795,
0.75605107239617,0.841327094176323,1.),(0.,0.840000000000002),
 .UNSPECIFIED.);
#188=B_SPLINE_SURFACE_WITH_KNOTS('',3,1,((#11581,#11582),(#11583,#11584),
(#11585,#11586),(#11587,#11588),(#11589,#11590),(#11591,#11592),(#11593,
#11594),(#11595,#11596),(#11597,#11598),(#11599,#11600),(#11601,#11602),
(#11603,#11604),(#11605,#11606),(#11607,#11608),(#11609,#11610),(#11611,
#11612),(#11613,#11614),(#11615,#11616),(#11617,#11618),(#11619,#11620),
(#11621,#11622),(#11623,#11624),(#11625,#11626)),.UNSPECIFIED.,.F.,.F.,
 .F.,(4,1,1,1,1,1,1,1,1,1,1,1,1,1,1,1,1,1,1,1,4),(2,2),(0.,0.158672905823676,
0.243948927603829,0.322402868082049,0.394034727302036,0.458844505321287,
0.516832202217594,0.567997818099863,0.612341353127269,0.649862807545807,
0.680562181765468,0.695323448997602,0.706670671285856,0.717793322185029,
0.728712887095513,0.760515567641419,0.791692515756145,0.823806980266354,
0.859359395195979,0.901681047937578,0.967654618228659),(0.,0.84),
 .UNSPECIFIED.);
#189=B_SPLINE_SURFACE_WITH_KNOTS('',3,1,((#11630,#11631),(#11632,#11633),
(#11634,#11635),(#11636,#11637),(#11638,#11639),(#11640,#11641),(#11642,
#11643),(#11644,#11645),(#11646,#11647),(#11648,#11649),(#11650,#11651),
(#11652,#11653),(#11654,#11655),(#11656,#11657),(#11658,#11659),(#11660,
#11661),(#11662,#11663),(#11664,#11665),(#11666,#11667),(#11668,#11669),
(#11670,#11671),(#11672,#11673),(#11674,#11675)),.UNSPECIFIED.,.F.,.F.,
 .F.,(4,1,1,1,1,1,1,1,1,1,1,1,1,1,1,1,1,1,1,1,4),(2,2),(0.0323453817713401,
0.0983189520624214,0.14064060480402,0.176193019733645,0.208307484243854,
0.23948443235858,0.271287112904486,0.28220667781497,0.293329328714142,0.304676551002397,
0.319437818234531,0.350137192454192,0.38765864687273,0.432002181900136,
0.483167797782405,0.541155494678712,0.605965272697963,0.67759713191795,
0.75605107239617,0.841327094176323,1.),(0.,0.84),.UNSPECIFIED.);
#190=B_SPLINE_SURFACE_WITH_KNOTS('',3,1,((#11679,#11680),(#11681,#11682),
(#11683,#11684),(#11685,#11686),(#11687,#11688),(#11689,#11690),(#11691,
#11692),(#11693,#11694),(#11695,#11696),(#11697,#11698),(#11699,#11700),
(#11701,#11702),(#11703,#11704),(#11705,#11706),(#11707,#11708),(#11709,
#11710),(#11711,#11712),(#11713,#11714),(#11715,#11716),(#11717,#11718),
(#11719,#11720),(#11721,#11722),(#11723,#11724)),.UNSPECIFIED.,.F.,.F.,
 .F.,(4,1,1,1,1,1,1,1,1,1,1,1,1,1,1,1,1,1,1,1,4),(2,2),(0.,0.158672905823676,
0.243948927603829,0.322402868082049,0.394034727302036,0.458844505321287,
0.516832202217594,0.567997818099863,0.612341353127269,0.649862807545807,
0.680562181765468,0.695323448997602,0.706670671285856,0.717793322185029,
0.728712887095513,0.760515567641419,0.791692515756145,0.823806980266354,
0.859359395195979,0.901681047937578,0.967654618228659),(0.,0.839999999999999),
 .UNSPECIFIED.);
#191=B_SPLINE_SURFACE_WITH_KNOTS('',3,1,((#11728,#11729),(#11730,#11731),
(#11732,#11733),(#11734,#11735),(#11736,#11737),(#11738,#11739),(#11740,
#11741),(#11742,#11743),(#11744,#11745),(#11746,#11747),(#11748,#11749),
(#11750,#11751),(#11752,#11753),(#11754,#11755),(#11756,#11757),(#11758,
#11759),(#11760,#11761),(#11762,#11763),(#11764,#11765),(#11766,#11767),
(#11768,#11769),(#11770,#11771),(#11772,#11773)),.UNSPECIFIED.,.F.,.F.,
 .F.,(4,1,1,1,1,1,1,1,1,1,1,1,1,1,1,1,1,1,1,1,4),(2,2),(0.0323453817713401,
0.0983189520624214,0.14064060480402,0.176193019733645,0.208307484243854,
0.23948443235858,0.271287112904486,0.28220667781497,0.293329328714142,0.304676551002397,
0.319437818234531,0.350137192454192,0.38765864687273,0.432002181900136,
0.483167797782405,0.541155494678712,0.605965272697963,0.67759713191795,
0.75605107239617,0.841327094176323,1.),(0.,0.839999999999998),
 .UNSPECIFIED.);
#192=B_SPLINE_SURFACE_WITH_KNOTS('',3,1,((#11777,#11778),(#11779,#11780),
(#11781,#11782),(#11783,#11784),(#11785,#11786),(#11787,#11788),(#11789,
#11790),(#11791,#11792),(#11793,#11794),(#11795,#11796),(#11797,#11798),
(#11799,#11800),(#11801,#11802),(#11803,#11804),(#11805,#11806),(#11807,
#11808),(#11809,#11810),(#11811,#11812),(#11813,#11814),(#11815,#11816),
(#11817,#11818),(#11819,#11820),(#11821,#11822)),.UNSPECIFIED.,.F.,.F.,
 .F.,(4,1,1,1,1,1,1,1,1,1,1,1,1,1,1,1,1,1,1,1,4),(2,2),(0.,0.158672905823676,
0.243948927603829,0.322402868082049,0.394034727302036,0.458844505321287,
0.516832202217594,0.567997818099863,0.612341353127269,0.649862807545807,
0.680562181765468,0.695323448997602,0.706670671285856,0.717793322185029,
0.728712887095513,0.760515567641419,0.791692515756145,0.823806980266354,
0.859359395195979,0.901681047937578,0.967654618228659),(0.,0.839999999999998),
 .UNSPECIFIED.);
#193=B_SPLINE_SURFACE_WITH_KNOTS('',3,1,((#11826,#11827),(#11828,#11829),
(#11830,#11831),(#11832,#11833),(#11834,#11835),(#11836,#11837),(#11838,
#11839),(#11840,#11841),(#11842,#11843),(#11844,#11845),(#11846,#11847),
(#11848,#11849),(#11850,#11851),(#11852,#11853),(#11854,#11855),(#11856,
#11857),(#11858,#11859),(#11860,#11861),(#11862,#11863),(#11864,#11865),
(#11866,#11867),(#11868,#11869),(#11870,#11871)),.UNSPECIFIED.,.F.,.F.,
 .F.,(4,1,1,1,1,1,1,1,1,1,1,1,1,1,1,1,1,1,1,1,4),(2,2),(0.0323453817713401,
0.0983189520624214,0.14064060480402,0.176193019733645,0.208307484243854,
0.23948443235858,0.271287112904486,0.28220667781497,0.293329328714142,0.304676551002397,
0.319437818234531,0.350137192454192,0.38765864687273,0.432002181900136,
0.483167797782405,0.541155494678712,0.605965272697963,0.67759713191795,
0.75605107239617,0.841327094176323,1.),(0.,0.839999999999998),
 .UNSPECIFIED.);
#194=B_SPLINE_SURFACE_WITH_KNOTS('',3,1,((#11875,#11876),(#11877,#11878),
(#11879,#11880),(#11881,#11882),(#11883,#11884),(#11885,#11886),(#11887,
#11888),(#11889,#11890),(#11891,#11892),(#11893,#11894),(#11895,#11896),
(#11897,#11898),(#11899,#11900),(#11901,#11902),(#11903,#11904),(#11905,
#11906),(#11907,#11908),(#11909,#11910),(#11911,#11912),(#11913,#11914),
(#11915,#11916),(#11917,#11918),(#11919,#11920)),.UNSPECIFIED.,.F.,.F.,
 .F.,(4,1,1,1,1,1,1,1,1,1,1,1,1,1,1,1,1,1,1,1,4),(2,2),(0.,0.158672905823676,
0.243948927603829,0.322402868082049,0.394034727302036,0.458844505321287,
0.516832202217594,0.567997818099863,0.612341353127269,0.649862807545807,
0.680562181765468,0.695323448997602,0.706670671285856,0.717793322185029,
0.728712887095513,0.760515567641419,0.791692515756145,0.823806980266354,
0.859359395195979,0.901681047937578,0.967654618228659),(0.,0.839999999999999),
 .UNSPECIFIED.);
#195=B_SPLINE_SURFACE_WITH_KNOTS('',3,1,((#11924,#11925),(#11926,#11927),
(#11928,#11929),(#11930,#11931),(#11932,#11933),(#11934,#11935),(#11936,
#11937),(#11938,#11939),(#11940,#11941),(#11942,#11943),(#11944,#11945),
(#11946,#11947),(#11948,#11949),(#11950,#11951),(#11952,#11953),(#11954,
#11955),(#11956,#11957),(#11958,#11959),(#11960,#11961),(#11962,#11963),
(#11964,#11965),(#11966,#11967),(#11968,#11969)),.UNSPECIFIED.,.F.,.F.,
 .F.,(4,1,1,1,1,1,1,1,1,1,1,1,1,1,1,1,1,1,1,1,4),(2,2),(0.0323453817713401,
0.0983189520624214,0.14064060480402,0.176193019733645,0.208307484243854,
0.23948443235858,0.271287112904486,0.28220667781497,0.293329328714142,0.304676551002397,
0.319437818234531,0.350137192454192,0.38765864687273,0.432002181900136,
0.483167797782405,0.541155494678712,0.605965272697963,0.67759713191795,
0.75605107239617,0.841327094176323,1.),(0.,0.84),.UNSPECIFIED.);
#196=B_SPLINE_SURFACE_WITH_KNOTS('',3,1,((#11973,#11974),(#11975,#11976),
(#11977,#11978),(#11979,#11980),(#11981,#11982),(#11983,#11984),(#11985,
#11986),(#11987,#11988),(#11989,#11990),(#11991,#11992),(#11993,#11994),
(#11995,#11996),(#11997,#11998),(#11999,#12000),(#12001,#12002),(#12003,
#12004),(#12005,#12006),(#12007,#12008),(#12009,#12010),(#12011,#12012),
(#12013,#12014),(#12015,#12016),(#12017,#12018)),.UNSPECIFIED.,.F.,.F.,
 .F.,(4,1,1,1,1,1,1,1,1,1,1,1,1,1,1,1,1,1,1,1,4),(2,2),(0.,0.158672905823676,
0.243948927603829,0.322402868082049,0.394034727302036,0.458844505321287,
0.516832202217594,0.567997818099863,0.612341353127269,0.649862807545807,
0.680562181765468,0.695323448997602,0.706670671285856,0.717793322185029,
0.728712887095513,0.760515567641419,0.791692515756145,0.823806980266354,
0.859359395195979,0.901681047937578,0.967654618228659),(0.,0.84),
 .UNSPECIFIED.);
#197=B_SPLINE_SURFACE_WITH_KNOTS('',3,1,((#12022,#12023),(#12024,#12025),
(#12026,#12027),(#12028,#12029),(#12030,#12031),(#12032,#12033),(#12034,
#12035),(#12036,#12037),(#12038,#12039),(#12040,#12041),(#12042,#12043),
(#12044,#12045),(#12046,#12047),(#12048,#12049),(#12050,#12051),(#12052,
#12053),(#12054,#12055),(#12056,#12057),(#12058,#12059),(#12060,#12061),
(#12062,#12063),(#12064,#12065),(#12066,#12067)),.UNSPECIFIED.,.F.,.F.,
 .F.,(4,1,1,1,1,1,1,1,1,1,1,1,1,1,1,1,1,1,1,1,4),(2,2),(0.0323453817713401,
0.0983189520624214,0.14064060480402,0.176193019733645,0.208307484243854,
0.23948443235858,0.271287112904486,0.28220667781497,0.293329328714142,0.304676551002397,
0.319437818234531,0.350137192454192,0.38765864687273,0.432002181900136,
0.483167797782405,0.541155494678712,0.605965272697963,0.67759713191795,
0.75605107239617,0.841327094176323,1.),(0.,0.84),.UNSPECIFIED.);
#198=B_SPLINE_SURFACE_WITH_KNOTS('',3,1,((#12071,#12072),(#12073,#12074),
(#12075,#12076),(#12077,#12078),(#12079,#12080),(#12081,#12082),(#12083,
#12084),(#12085,#12086),(#12087,#12088),(#12089,#12090),(#12091,#12092),
(#12093,#12094),(#12095,#12096),(#12097,#12098),(#12099,#12100),(#12101,
#12102),(#12103,#12104),(#12105,#12106),(#12107,#12108),(#12109,#12110),
(#12111,#12112),(#12113,#12114),(#12115,#12116)),.UNSPECIFIED.,.F.,.F.,
 .F.,(4,1,1,1,1,1,1,1,1,1,1,1,1,1,1,1,1,1,1,1,4),(2,2),(0.,0.158672905823676,
0.243948927603829,0.322402868082049,0.394034727302036,0.458844505321287,
0.516832202217594,0.567997818099863,0.612341353127269,0.649862807545807,
0.680562181765468,0.695323448997602,0.706670671285856,0.717793322185029,
0.728712887095513,0.760515567641419,0.791692515756145,0.823806980266354,
0.859359395195979,0.901681047937578,0.967654618228659),(0.,0.839999999999999),
 .UNSPECIFIED.);
#199=B_SPLINE_SURFACE_WITH_KNOTS('',3,1,((#12120,#12121),(#12122,#12123),
(#12124,#12125),(#12126,#12127),(#12128,#12129),(#12130,#12131),(#12132,
#12133),(#12134,#12135),(#12136,#12137),(#12138,#12139),(#12140,#12141),
(#12142,#12143),(#12144,#12145),(#12146,#12147),(#12148,#12149),(#12150,
#12151),(#12152,#12153),(#12154,#12155),(#12156,#12157),(#12158,#12159),
(#12160,#12161),(#12162,#12163),(#12164,#12165)),.UNSPECIFIED.,.F.,.F.,
 .F.,(4,1,1,1,1,1,1,1,1,1,1,1,1,1,1,1,1,1,1,1,4),(2,2),(0.0323453817713401,
0.0983189520624214,0.14064060480402,0.176193019733645,0.208307484243854,
0.23948443235858,0.271287112904486,0.28220667781497,0.293329328714142,0.304676551002397,
0.319437818234531,0.350137192454192,0.38765864687273,0.432002181900136,
0.483167797782405,0.541155494678712,0.605965272697963,0.67759713191795,
0.75605107239617,0.841327094176323,1.),(0.,0.84),.UNSPECIFIED.);
#200=B_SPLINE_SURFACE_WITH_KNOTS('',3,1,((#12169,#12170),(#12171,#12172),
(#12173,#12174),(#12175,#12176),(#12177,#12178),(#12179,#12180),(#12181,
#12182),(#12183,#12184),(#12185,#12186),(#12187,#12188),(#12189,#12190),
(#12191,#12192),(#12193,#12194),(#12195,#12196),(#12197,#12198),(#12199,
#12200),(#12201,#12202),(#12203,#12204),(#12205,#12206),(#12207,#12208),
(#12209,#12210),(#12211,#12212),(#12213,#12214)),.UNSPECIFIED.,.F.,.F.,
 .F.,(4,1,1,1,1,1,1,1,1,1,1,1,1,1,1,1,1,1,1,1,4),(2,2),(0.,0.158672905823676,
0.243948927603829,0.322402868082049,0.394034727302036,0.458844505321287,
0.516832202217594,0.567997818099863,0.612341353127269,0.649862807545807,
0.680562181765468,0.695323448997602,0.706670671285856,0.717793322185029,
0.728712887095513,0.760515567641419,0.791692515756145,0.823806980266354,
0.859359395195979,0.901681047937578,0.967654618228659),(0.,0.84),
 .UNSPECIFIED.);
#201=B_SPLINE_SURFACE_WITH_KNOTS('',3,1,((#12218,#12219),(#12220,#12221),
(#12222,#12223),(#12224,#12225),(#12226,#12227),(#12228,#12229),(#12230,
#12231),(#12232,#12233),(#12234,#12235),(#12236,#12237),(#12238,#12239),
(#12240,#12241),(#12242,#12243),(#12244,#12245),(#12246,#12247),(#12248,
#12249),(#12250,#12251),(#12252,#12253),(#12254,#12255),(#12256,#12257),
(#12258,#12259),(#12260,#12261),(#12262,#12263)),.UNSPECIFIED.,.F.,.F.,
 .F.,(4,1,1,1,1,1,1,1,1,1,1,1,1,1,1,1,1,1,1,1,4),(2,2),(0.0323453817713401,
0.0983189520624214,0.14064060480402,0.176193019733645,0.208307484243854,
0.23948443235858,0.271287112904486,0.28220667781497,0.293329328714142,0.304676551002397,
0.319437818234531,0.350137192454192,0.38765864687273,0.432002181900136,
0.483167797782405,0.541155494678712,0.605965272697963,0.67759713191795,
0.75605107239617,0.841327094176323,1.),(0.,0.839999999999998),
 .UNSPECIFIED.);
#202=B_SPLINE_SURFACE_WITH_KNOTS('',3,1,((#12267,#12268),(#12269,#12270),
(#12271,#12272),(#12273,#12274),(#12275,#12276),(#12277,#12278),(#12279,
#12280),(#12281,#12282),(#12283,#12284),(#12285,#12286),(#12287,#12288),
(#12289,#12290),(#12291,#12292),(#12293,#12294),(#12295,#12296),(#12297,
#12298),(#12299,#12300),(#12301,#12302),(#12303,#12304),(#12305,#12306),
(#12307,#12308),(#12309,#12310),(#12311,#12312)),.UNSPECIFIED.,.F.,.F.,
 .F.,(4,1,1,1,1,1,1,1,1,1,1,1,1,1,1,1,1,1,1,1,4),(2,2),(0.,0.158672905823676,
0.243948927603829,0.322402868082049,0.394034727302036,0.458844505321287,
0.516832202217594,0.567997818099863,0.612341353127269,0.649862807545807,
0.680562181765468,0.695323448997602,0.706670671285856,0.717793322185029,
0.728712887095513,0.760515567641419,0.791692515756145,0.823806980266354,
0.859359395195979,0.901681047937578,0.967654618228659),(0.,0.839999999999999),
 .UNSPECIFIED.);
#203=B_SPLINE_SURFACE_WITH_KNOTS('',3,1,((#12316,#12317),(#12318,#12319),
(#12320,#12321),(#12322,#12323),(#12324,#12325),(#12326,#12327),(#12328,
#12329),(#12330,#12331),(#12332,#12333),(#12334,#12335),(#12336,#12337),
(#12338,#12339),(#12340,#12341),(#12342,#12343),(#12344,#12345),(#12346,
#12347),(#12348,#12349),(#12350,#12351),(#12352,#12353),(#12354,#12355),
(#12356,#12357),(#12358,#12359),(#12360,#12361)),.UNSPECIFIED.,.F.,.F.,
 .F.,(4,1,1,1,1,1,1,1,1,1,1,1,1,1,1,1,1,1,1,1,4),(2,2),(0.0323453817713401,
0.0983189520624214,0.14064060480402,0.176193019733645,0.208307484243854,
0.23948443235858,0.271287112904486,0.28220667781497,0.293329328714142,0.304676551002397,
0.319437818234531,0.350137192454192,0.38765864687273,0.432002181900136,
0.483167797782405,0.541155494678712,0.605965272697963,0.67759713191795,
0.75605107239617,0.841327094176323,1.),(0.,0.84),.UNSPECIFIED.);
#204=B_SPLINE_SURFACE_WITH_KNOTS('',3,1,((#12365,#12366),(#12367,#12368),
(#12369,#12370),(#12371,#12372),(#12373,#12374),(#12375,#12376),(#12377,
#12378),(#12379,#12380),(#12381,#12382),(#12383,#12384),(#12385,#12386),
(#12387,#12388),(#12389,#12390),(#12391,#12392),(#12393,#12394),(#12395,
#12396),(#12397,#12398),(#12399,#12400),(#12401,#12402),(#12403,#12404),
(#12405,#12406),(#12407,#12408),(#12409,#12410)),.UNSPECIFIED.,.F.,.F.,
 .F.,(4,1,1,1,1,1,1,1,1,1,1,1,1,1,1,1,1,1,1,1,4),(2,2),(0.,0.158672905823676,
0.243948927603829,0.322402868082049,0.394034727302036,0.458844505321287,
0.516832202217594,0.567997818099863,0.612341353127269,0.649862807545807,
0.680562181765468,0.695323448997602,0.706670671285856,0.717793322185029,
0.728712887095513,0.760515567641419,0.791692515756145,0.823806980266354,
0.859359395195979,0.901681047937578,0.967654618228659),(0.,0.839999999999999),
 .UNSPECIFIED.);
#205=B_SPLINE_SURFACE_WITH_KNOTS('',3,1,((#12414,#12415),(#12416,#12417),
(#12418,#12419),(#12420,#12421),(#12422,#12423),(#12424,#12425),(#12426,
#12427),(#12428,#12429),(#12430,#12431),(#12432,#12433),(#12434,#12435),
(#12436,#12437),(#12438,#12439),(#12440,#12441),(#12442,#12443),(#12444,
#12445),(#12446,#12447),(#12448,#12449),(#12450,#12451),(#12452,#12453),
(#12454,#12455),(#12456,#12457),(#12458,#12459)),.UNSPECIFIED.,.F.,.F.,
 .F.,(4,1,1,1,1,1,1,1,1,1,1,1,1,1,1,1,1,1,1,1,4),(2,2),(0.0323453817713401,
0.0983189520624214,0.14064060480402,0.176193019733645,0.208307484243854,
0.23948443235858,0.271287112904486,0.28220667781497,0.293329328714142,0.304676551002397,
0.319437818234531,0.350137192454192,0.38765864687273,0.432002181900136,
0.483167797782405,0.541155494678712,0.605965272697963,0.67759713191795,
0.75605107239617,0.841327094176323,1.),(0.,0.84),.UNSPECIFIED.);
#206=B_SPLINE_SURFACE_WITH_KNOTS('',3,1,((#12463,#12464),(#12465,#12466),
(#12467,#12468),(#12469,#12470),(#12471,#12472),(#12473,#12474),(#12475,
#12476),(#12477,#12478),(#12479,#12480),(#12481,#12482),(#12483,#12484),
(#12485,#12486),(#12487,#12488),(#12489,#12490),(#12491,#12492),(#12493,
#12494),(#12495,#12496),(#12497,#12498),(#12499,#12500),(#12501,#12502),
(#12503,#12504),(#12505,#12506),(#12507,#12508)),.UNSPECIFIED.,.F.,.F.,
 .F.,(4,1,1,1,1,1,1,1,1,1,1,1,1,1,1,1,1,1,1,1,4),(2,2),(0.,0.158672905823676,
0.243948927603829,0.322402868082049,0.394034727302036,0.458844505321287,
0.516832202217594,0.567997818099863,0.612341353127269,0.649862807545807,
0.680562181765468,0.695323448997602,0.706670671285856,0.717793322185029,
0.728712887095513,0.760515567641419,0.791692515756145,0.823806980266354,
0.859359395195979,0.901681047937578,0.967654618228659),(0.,0.839999999999999),
 .UNSPECIFIED.);
#207=B_SPLINE_CURVE_WITH_KNOTS('',3,(#8481,#8482,#8483,#8484,#8485,#8486,
#8487,#8488,#8489,#8490,#8491,#8492,#8493,#8494,#8495,#8496,#8497,#8498,
#8499,#8500,#8501,#8502,#8503),.UNSPECIFIED.,.F.,.F.,(4,1,1,1,1,1,1,1,1,
1,1,1,1,1,1,1,1,1,1,1,4),(0.0323453817713401,0.0983189520624214,0.14064060480402,
0.176193019733645,0.208307484243854,0.23948443235858,0.271287112904486,
0.28220667781497,0.293329328714142,0.304676551002397,0.319437818234531,
0.350137192454192,0.38765864687273,0.432002181900136,0.483167797782405,
0.541155494678712,0.605965272697963,0.67759713191795,0.75605107239617,0.841327094176323,
1.),.UNSPECIFIED.);
#208=B_SPLINE_CURVE_WITH_KNOTS('',3,(#8507,#8508,#8509,#8510,#8511,#8512,
#8513,#8514,#8515,#8516,#8517,#8518,#8519,#8520,#8521,#8522,#8523,#8524,
#8525,#8526,#8527,#8528,#8529),.UNSPECIFIED.,.F.,.F.,(4,1,1,1,1,1,1,1,1,
1,1,1,1,1,1,1,1,1,1,1,4),(0.,0.158672905823676,0.243948927603829,0.322402868082049,
0.394034727302036,0.458844505321287,0.516832202217594,0.567997818099863,
0.612341353127269,0.649862807545807,0.680562181765468,0.695323448997602,
0.706670671285856,0.717793322185029,0.728712887095513,0.760515567641419,
0.791692515756145,0.823806980266354,0.859359395195979,0.901681047937578,
0.967654618228659),.UNSPECIFIED.);
#209=B_SPLINE_CURVE_WITH_KNOTS('',3,(#8533,#8534,#8535,#8536,#8537,#8538,
#8539,#8540,#8541,#8542,#8543,#8544,#8545,#8546,#8547,#8548,#8549,#8550,
#8551,#8552,#8553,#8554,#8555),.UNSPECIFIED.,.F.,.F.,(4,1,1,1,1,1,1,1,1,
1,1,1,1,1,1,1,1,1,1,1,4),(0.0323453817713401,0.0983189520624214,0.14064060480402,
0.176193019733645,0.208307484243854,0.23948443235858,0.271287112904486,
0.28220667781497,0.293329328714142,0.304676551002397,0.319437818234531,
0.350137192454192,0.38765864687273,0.432002181900136,0.483167797782405,
0.541155494678712,0.605965272697963,0.67759713191795,0.75605107239617,0.841327094176323,
1.),.UNSPECIFIED.);
#210=B_SPLINE_CURVE_WITH_KNOTS('',3,(#8559,#8560,#8561,#8562,#8563,#8564,
#8565,#8566,#8567,#8568,#8569,#8570,#8571,#8572,#8573,#8574,#8575,#8576,
#8577,#8578,#8579,#8580,#8581),.UNSPECIFIED.,.F.,.F.,(4,1,1,1,1,1,1,1,1,
1,1,1,1,1,1,1,1,1,1,1,4),(0.,0.158672905823676,0.243948927603829,0.322402868082049,
0.394034727302036,0.458844505321287,0.516832202217594,0.567997818099863,
0.612341353127269,0.649862807545807,0.680562181765468,0.695323448997602,
0.706670671285856,0.717793322185029,0.728712887095513,0.760515567641419,
0.791692515756145,0.823806980266354,0.859359395195979,0.901681047937578,
0.967654618228659),.UNSPECIFIED.);
#211=B_SPLINE_CURVE_WITH_KNOTS('',3,(#8585,#8586,#8587,#8588,#8589,#8590,
#8591,#8592,#8593,#8594,#8595,#8596,#8597,#8598,#8599,#8600,#8601,#8602,
#8603,#8604,#8605,#8606,#8607),.UNSPECIFIED.,.F.,.F.,(4,1,1,1,1,1,1,1,1,
1,1,1,1,1,1,1,1,1,1,1,4),(0.0323453817713401,0.0983189520624214,0.14064060480402,
0.176193019733645,0.208307484243854,0.23948443235858,0.271287112904486,
0.28220667781497,0.293329328714142,0.304676551002397,0.319437818234531,
0.350137192454192,0.38765864687273,0.432002181900136,0.483167797782405,
0.541155494678712,0.605965272697963,0.67759713191795,0.75605107239617,0.841327094176323,
1.),.UNSPECIFIED.);
#212=B_SPLINE_CURVE_WITH_KNOTS('',3,(#8611,#8612,#8613,#8614,#8615,#8616,
#8617,#8618,#8619,#8620,#8621,#8622,#8623,#8624,#8625,#8626,#8627,#8628,
#8629,#8630,#8631,#8632,#8633),.UNSPECIFIED.,.F.,.F.,(4,1,1,1,1,1,1,1,1,
1,1,1,1,1,1,1,1,1,1,1,4),(0.,0.158672905823676,0.243948927603829,0.322402868082049,
0.394034727302036,0.458844505321287,0.516832202217594,0.567997818099863,
0.612341353127269,0.649862807545807,0.680562181765468,0.695323448997602,
0.706670671285856,0.717793322185029,0.728712887095513,0.760515567641419,
0.791692515756145,0.823806980266354,0.859359395195979,0.901681047937578,
0.967654618228659),.UNSPECIFIED.);
#213=B_SPLINE_CURVE_WITH_KNOTS('',3,(#8637,#8638,#8639,#8640,#8641,#8642,
#8643,#8644,#8645,#8646,#8647,#8648,#8649,#8650,#8651,#8652,#8653,#8654,
#8655,#8656,#8657,#8658,#8659),.UNSPECIFIED.,.F.,.F.,(4,1,1,1,1,1,1,1,1,
1,1,1,1,1,1,1,1,1,1,1,4),(0.0323453817713401,0.0983189520624214,0.14064060480402,
0.176193019733645,0.208307484243854,0.23948443235858,0.271287112904486,
0.28220667781497,0.293329328714142,0.304676551002397,0.319437818234531,
0.350137192454192,0.38765864687273,0.432002181900136,0.483167797782405,
0.541155494678712,0.605965272697963,0.67759713191795,0.75605107239617,0.841327094176323,
1.),.UNSPECIFIED.);
#214=B_SPLINE_CURVE_WITH_KNOTS('',3,(#8663,#8664,#8665,#8666,#8667,#8668,
#8669,#8670,#8671,#8672,#8673,#8674,#8675,#8676,#8677,#8678,#8679,#8680,
#8681,#8682,#8683,#8684,#8685),.UNSPECIFIED.,.F.,.F.,(4,1,1,1,1,1,1,1,1,
1,1,1,1,1,1,1,1,1,1,1,4),(0.,0.158672905823676,0.243948927603829,0.322402868082049,
0.394034727302036,0.458844505321287,0.516832202217594,0.567997818099863,
0.612341353127269,0.649862807545807,0.680562181765468,0.695323448997602,
0.706670671285856,0.717793322185029,0.728712887095513,0.760515567641419,
0.791692515756145,0.823806980266354,0.859359395195979,0.901681047937578,
0.967654618228659),.UNSPECIFIED.);
#215=B_SPLINE_CURVE_WITH_KNOTS('',3,(#8689,#8690,#8691,#8692,#8693,#8694,
#8695,#8696,#8697,#8698,#8699,#8700,#8701,#8702,#8703,#8704,#8705,#8706,
#8707,#8708,#8709,#8710,#8711),.UNSPECIFIED.,.F.,.F.,(4,1,1,1,1,1,1,1,1,
1,1,1,1,1,1,1,1,1,1,1,4),(0.0323453817713401,0.0983189520624214,0.14064060480402,
0.176193019733645,0.208307484243854,0.23948443235858,0.271287112904486,
0.28220667781497,0.293329328714142,0.304676551002397,0.319437818234531,
0.350137192454192,0.38765864687273,0.432002181900136,0.483167797782405,
0.541155494678712,0.605965272697963,0.67759713191795,0.75605107239617,0.841327094176323,
1.),.UNSPECIFIED.);
#216=B_SPLINE_CURVE_WITH_KNOTS('',3,(#8715,#8716,#8717,#8718,#8719,#8720,
#8721,#8722,#8723,#8724,#8725,#8726,#8727,#8728,#8729,#8730,#8731,#8732,
#8733,#8734,#8735,#8736,#8737),.UNSPECIFIED.,.F.,.F.,(4,1,1,1,1,1,1,1,1,
1,1,1,1,1,1,1,1,1,1,1,4),(0.,0.158672905823676,0.243948927603829,0.322402868082049,
0.394034727302036,0.458844505321287,0.516832202217594,0.567997818099863,
0.612341353127269,0.649862807545807,0.680562181765468,0.695323448997602,
0.706670671285856,0.717793322185029,0.728712887095513,0.760515567641419,
0.791692515756145,0.823806980266354,0.859359395195979,0.901681047937578,
0.967654618228659),.UNSPECIFIED.);
#217=B_SPLINE_CURVE_WITH_KNOTS('',3,(#8741,#8742,#8743,#8744,#8745,#8746,
#8747,#8748,#8749,#8750,#8751,#8752,#8753,#8754,#8755,#8756,#8757,#8758,
#8759,#8760,#8761,#8762,#8763),.UNSPECIFIED.,.F.,.F.,(4,1,1,1,1,1,1,1,1,
1,1,1,1,1,1,1,1,1,1,1,4),(0.0323453817713401,0.0983189520624214,0.14064060480402,
0.176193019733645,0.208307484243854,0.23948443235858,0.271287112904486,
0.28220667781497,0.293329328714142,0.304676551002397,0.319437818234531,
0.350137192454192,0.38765864687273,0.432002181900136,0.483167797782405,
0.541155494678712,0.605965272697963,0.67759713191795,0.75605107239617,0.841327094176323,
1.),.UNSPECIFIED.);
#218=B_SPLINE_CURVE_WITH_KNOTS('',3,(#8767,#8768,#8769,#8770,#8771,#8772,
#8773,#8774,#8775,#8776,#8777,#8778,#8779,#8780,#8781,#8782,#8783,#8784,
#8785,#8786,#8787,#8788,#8789),.UNSPECIFIED.,.F.,.F.,(4,1,1,1,1,1,1,1,1,
1,1,1,1,1,1,1,1,1,1,1,4),(0.,0.158672905823676,0.243948927603829,0.322402868082049,
0.394034727302036,0.458844505321287,0.516832202217594,0.567997818099863,
0.612341353127269,0.649862807545807,0.680562181765468,0.695323448997602,
0.706670671285856,0.717793322185029,0.728712887095513,0.760515567641419,
0.791692515756145,0.823806980266354,0.859359395195979,0.901681047937578,
0.967654618228659),.UNSPECIFIED.);
#219=B_SPLINE_CURVE_WITH_KNOTS('',3,(#8793,#8794,#8795,#8796,#8797,#8798,
#8799,#8800,#8801,#8802,#8803,#8804,#8805,#8806,#8807,#8808,#8809,#8810,
#8811,#8812,#8813,#8814,#8815),.UNSPECIFIED.,.F.,.F.,(4,1,1,1,1,1,1,1,1,
1,1,1,1,1,1,1,1,1,1,1,4),(0.0323453817713401,0.0983189520624214,0.14064060480402,
0.176193019733645,0.208307484243854,0.23948443235858,0.271287112904486,
0.28220667781497,0.293329328714142,0.304676551002397,0.319437818234531,
0.350137192454192,0.38765864687273,0.432002181900136,0.483167797782405,
0.541155494678712,0.605965272697963,0.67759713191795,0.75605107239617,0.841327094176323,
1.),.UNSPECIFIED.);
#220=B_SPLINE_CURVE_WITH_KNOTS('',3,(#8819,#8820,#8821,#8822,#8823,#8824,
#8825,#8826,#8827,#8828,#8829,#8830,#8831,#8832,#8833,#8834,#8835,#8836,
#8837,#8838,#8839,#8840,#8841),.UNSPECIFIED.,.F.,.F.,(4,1,1,1,1,1,1,1,1,
1,1,1,1,1,1,1,1,1,1,1,4),(0.,0.158672905823676,0.243948927603829,0.322402868082049,
0.394034727302036,0.458844505321287,0.516832202217594,0.567997818099863,
0.612341353127269,0.649862807545807,0.680562181765468,0.695323448997602,
0.706670671285856,0.717793322185029,0.728712887095513,0.760515567641419,
0.791692515756145,0.823806980266354,0.859359395195979,0.901681047937578,
0.967654618228659),.UNSPECIFIED.);
#221=B_SPLINE_CURVE_WITH_KNOTS('',3,(#8845,#8846,#8847,#8848,#8849,#8850,
#8851,#8852,#8853,#8854,#8855,#8856,#8857,#8858,#8859,#8860,#8861,#8862,
#8863,#8864,#8865,#8866,#8867),.UNSPECIFIED.,.F.,.F.,(4,1,1,1,1,1,1,1,1,
1,1,1,1,1,1,1,1,1,1,1,4),(0.0323453817713401,0.0983189520624214,0.14064060480402,
0.176193019733645,0.208307484243854,0.23948443235858,0.271287112904486,
0.28220667781497,0.293329328714142,0.304676551002397,0.319437818234531,
0.350137192454192,0.38765864687273,0.432002181900136,0.483167797782405,
0.541155494678712,0.605965272697963,0.67759713191795,0.75605107239617,0.841327094176323,
1.),.UNSPECIFIED.);
#222=B_SPLINE_CURVE_WITH_KNOTS('',3,(#8871,#8872,#8873,#8874,#8875,#8876,
#8877,#8878,#8879,#8880,#8881,#8882,#8883,#8884,#8885,#8886,#8887,#8888,
#8889,#8890,#8891,#8892,#8893),.UNSPECIFIED.,.F.,.F.,(4,1,1,1,1,1,1,1,1,
1,1,1,1,1,1,1,1,1,1,1,4),(0.,0.158672905823676,0.243948927603829,0.322402868082049,
0.394034727302036,0.458844505321287,0.516832202217594,0.567997818099863,
0.612341353127269,0.649862807545807,0.680562181765468,0.695323448997602,
0.706670671285856,0.717793322185029,0.728712887095513,0.760515567641419,
0.791692515756145,0.823806980266354,0.859359395195979,0.901681047937578,
0.967654618228659),.UNSPECIFIED.);
#223=B_SPLINE_CURVE_WITH_KNOTS('',3,(#8897,#8898,#8899,#8900,#8901,#8902,
#8903,#8904,#8905,#8906,#8907,#8908,#8909,#8910,#8911,#8912,#8913,#8914,
#8915,#8916,#8917,#8918,#8919),.UNSPECIFIED.,.F.,.F.,(4,1,1,1,1,1,1,1,1,
1,1,1,1,1,1,1,1,1,1,1,4),(0.0323453817713401,0.0983189520624214,0.14064060480402,
0.176193019733645,0.208307484243854,0.23948443235858,0.271287112904486,
0.28220667781497,0.293329328714142,0.304676551002397,0.319437818234531,
0.350137192454192,0.38765864687273,0.432002181900136,0.483167797782405,
0.541155494678712,0.605965272697963,0.67759713191795,0.75605107239617,0.841327094176323,
1.),.UNSPECIFIED.);
#224=B_SPLINE_CURVE_WITH_KNOTS('',3,(#8922,#8923,#8924,#8925,#8926,#8927,
#8928,#8929,#8930,#8931,#8932,#8933,#8934,#8935,#8936,#8937,#8938,#8939,
#8940,#8941,#8942,#8943,#8944),.UNSPECIFIED.,.F.,.F.,(4,1,1,1,1,1,1,1,1,
1,1,1,1,1,1,1,1,1,1,1,4),(0.,0.158672905823676,0.243948927603829,0.322402868082049,
0.394034727302036,0.458844505321287,0.516832202217594,0.567997818099863,
0.612341353127269,0.649862807545807,0.680562181765468,0.695323448997602,
0.706670671285856,0.717793322185029,0.728712887095513,0.760515567641419,
0.791692515756145,0.823806980266354,0.859359395195979,0.901681047937578,
0.967654618228659),.UNSPECIFIED.);
#225=B_SPLINE_CURVE_WITH_KNOTS('',3,(#8946,#8947,#8948,#8949,#8950,#8951,
#8952,#8953,#8954,#8955,#8956,#8957,#8958,#8959,#8960,#8961,#8962,#8963,
#8964,#8965,#8966,#8967,#8968),.UNSPECIFIED.,.F.,.F.,(4,1,1,1,1,1,1,1,1,
1,1,1,1,1,1,1,1,1,1,1,4),(0.0323453817713401,0.0983189520624214,0.14064060480402,
0.176193019733645,0.208307484243854,0.23948443235858,0.271287112904486,
0.28220667781497,0.293329328714142,0.304676551002397,0.319437818234531,
0.350137192454192,0.38765864687273,0.432002181900136,0.483167797782405,
0.541155494678712,0.605965272697963,0.67759713191795,0.75605107239617,0.841327094176323,
1.),.UNSPECIFIED.);
#226=B_SPLINE_CURVE_WITH_KNOTS('',3,(#8972,#8973,#8974,#8975,#8976,#8977,
#8978,#8979,#8980,#8981,#8982,#8983,#8984,#8985,#8986,#8987,#8988,#8989,
#8990,#8991,#8992,#8993,#8994),.UNSPECIFIED.,.F.,.F.,(4,1,1,1,1,1,1,1,1,
1,1,1,1,1,1,1,1,1,1,1,4),(0.,0.158672905823676,0.243948927603829,0.322402868082049,
0.394034727302036,0.458844505321287,0.516832202217594,0.567997818099863,
0.612341353127269,0.649862807545807,0.680562181765468,0.695323448997602,
0.706670671285856,0.717793322185029,0.728712887095513,0.760515567641419,
0.791692515756145,0.823806980266354,0.859359395195979,0.901681047937578,
0.967654618228659),.UNSPECIFIED.);
#227=B_SPLINE_CURVE_WITH_KNOTS('',3,(#8998,#8999,#9000,#9001,#9002,#9003,
#9004,#9005,#9006,#9007,#9008,#9009,#9010,#9011,#9012,#9013,#9014,#9015,
#9016,#9017,#9018,#9019,#9020),.UNSPECIFIED.,.F.,.F.,(4,1,1,1,1,1,1,1,1,
1,1,1,1,1,1,1,1,1,1,1,4),(0.0323453817713401,0.0983189520624214,0.14064060480402,
0.176193019733645,0.208307484243854,0.23948443235858,0.271287112904486,
0.28220667781497,0.293329328714142,0.304676551002397,0.319437818234531,
0.350137192454192,0.38765864687273,0.432002181900136,0.483167797782405,
0.541155494678712,0.605965272697963,0.67759713191795,0.75605107239617,0.841327094176323,
1.),.UNSPECIFIED.);
#228=B_SPLINE_CURVE_WITH_KNOTS('',3,(#9024,#9025,#9026,#9027,#9028,#9029,
#9030,#9031,#9032,#9033,#9034,#9035,#9036,#9037,#9038,#9039,#9040,#9041,
#9042,#9043,#9044,#9045,#9046),.UNSPECIFIED.,.F.,.F.,(4,1,1,1,1,1,1,1,1,
1,1,1,1,1,1,1,1,1,1,1,4),(0.,0.158672905823676,0.243948927603829,0.322402868082049,
0.394034727302036,0.458844505321287,0.516832202217594,0.567997818099863,
0.612341353127269,0.649862807545807,0.680562181765468,0.695323448997602,
0.706670671285856,0.717793322185029,0.728712887095513,0.760515567641419,
0.791692515756145,0.823806980266354,0.859359395195979,0.901681047937578,
0.967654618228659),.UNSPECIFIED.);
#229=B_SPLINE_CURVE_WITH_KNOTS('',3,(#9050,#9051,#9052,#9053,#9054,#9055,
#9056,#9057,#9058,#9059,#9060,#9061,#9062,#9063,#9064,#9065,#9066,#9067,
#9068,#9069,#9070,#9071,#9072),.UNSPECIFIED.,.F.,.F.,(4,1,1,1,1,1,1,1,1,
1,1,1,1,1,1,1,1,1,1,1,4),(0.0323453817713401,0.0983189520624214,0.14064060480402,
0.176193019733645,0.208307484243854,0.23948443235858,0.271287112904486,
0.28220667781497,0.293329328714142,0.304676551002397,0.319437818234531,
0.350137192454192,0.38765864687273,0.432002181900136,0.483167797782405,
0.541155494678712,0.605965272697963,0.67759713191795,0.75605107239617,0.841327094176323,
1.),.UNSPECIFIED.);
#230=B_SPLINE_CURVE_WITH_KNOTS('',3,(#9076,#9077,#9078,#9079,#9080,#9081,
#9082,#9083,#9084,#9085,#9086,#9087,#9088,#9089,#9090,#9091,#9092,#9093,
#9094,#9095,#9096,#9097,#9098),.UNSPECIFIED.,.F.,.F.,(4,1,1,1,1,1,1,1,1,
1,1,1,1,1,1,1,1,1,1,1,4),(0.,0.158672905823676,0.243948927603829,0.322402868082049,
0.394034727302036,0.458844505321287,0.516832202217594,0.567997818099863,
0.612341353127269,0.649862807545807,0.680562181765468,0.695323448997602,
0.706670671285856,0.717793322185029,0.728712887095513,0.760515567641419,
0.791692515756145,0.823806980266354,0.859359395195979,0.901681047937578,
0.967654618228659),.UNSPECIFIED.);
#231=B_SPLINE_CURVE_WITH_KNOTS('',3,(#9102,#9103,#9104,#9105,#9106,#9107,
#9108,#9109,#9110,#9111,#9112,#9113,#9114,#9115,#9116,#9117,#9118,#9119,
#9120,#9121,#9122,#9123,#9124),.UNSPECIFIED.,.F.,.F.,(4,1,1,1,1,1,1,1,1,
1,1,1,1,1,1,1,1,1,1,1,4),(0.0323453817713401,0.0983189520624214,0.14064060480402,
0.176193019733645,0.208307484243854,0.23948443235858,0.271287112904486,
0.28220667781497,0.293329328714142,0.304676551002397,0.319437818234531,
0.350137192454192,0.38765864687273,0.432002181900136,0.483167797782405,
0.541155494678712,0.605965272697963,0.67759713191795,0.75605107239617,0.841327094176323,
1.),.UNSPECIFIED.);
#232=B_SPLINE_CURVE_WITH_KNOTS('',3,(#9128,#9129,#9130,#9131,#9132,#9133,
#9134,#9135,#9136,#9137,#9138,#9139,#9140,#9141,#9142,#9143,#9144,#9145,
#9146,#9147,#9148,#9149,#9150),.UNSPECIFIED.,.F.,.F.,(4,1,1,1,1,1,1,1,1,
1,1,1,1,1,1,1,1,1,1,1,4),(0.,0.158672905823676,0.243948927603829,0.322402868082049,
0.394034727302036,0.458844505321287,0.516832202217594,0.567997818099863,
0.612341353127269,0.649862807545807,0.680562181765468,0.695323448997602,
0.706670671285856,0.717793322185029,0.728712887095513,0.760515567641419,
0.791692515756145,0.823806980266354,0.859359395195979,0.901681047937578,
0.967654618228659),.UNSPECIFIED.);
#233=B_SPLINE_CURVE_WITH_KNOTS('',3,(#9154,#9155,#9156,#9157,#9158,#9159,
#9160,#9161,#9162,#9163,#9164,#9165,#9166,#9167,#9168,#9169,#9170,#9171,
#9172,#9173,#9174,#9175,#9176),.UNSPECIFIED.,.F.,.F.,(4,1,1,1,1,1,1,1,1,
1,1,1,1,1,1,1,1,1,1,1,4),(0.0323453817713401,0.0983189520624214,0.14064060480402,
0.176193019733645,0.208307484243854,0.23948443235858,0.271287112904486,
0.28220667781497,0.293329328714142,0.304676551002397,0.319437818234531,
0.350137192454192,0.38765864687273,0.432002181900136,0.483167797782405,
0.541155494678712,0.605965272697963,0.67759713191795,0.75605107239617,0.841327094176323,
1.),.UNSPECIFIED.);
#234=B_SPLINE_CURVE_WITH_KNOTS('',3,(#9180,#9181,#9182,#9183,#9184,#9185,
#9186,#9187,#9188,#9189,#9190,#9191,#9192,#9193,#9194,#9195,#9196,#9197,
#9198,#9199,#9200,#9201,#9202),.UNSPECIFIED.,.F.,.F.,(4,1,1,1,1,1,1,1,1,
1,1,1,1,1,1,1,1,1,1,1,4),(0.,0.158672905823676,0.243948927603829,0.322402868082049,
0.394034727302036,0.458844505321287,0.516832202217594,0.567997818099863,
0.612341353127269,0.649862807545807,0.680562181765468,0.695323448997602,
0.706670671285856,0.717793322185029,0.728712887095513,0.760515567641419,
0.791692515756145,0.823806980266354,0.859359395195979,0.901681047937578,
0.967654618228659),.UNSPECIFIED.);
#235=B_SPLINE_CURVE_WITH_KNOTS('',3,(#9206,#9207,#9208,#9209,#9210,#9211,
#9212,#9213,#9214,#9215,#9216,#9217,#9218,#9219,#9220,#9221,#9222,#9223,
#9224,#9225,#9226,#9227,#9228),.UNSPECIFIED.,.F.,.F.,(4,1,1,1,1,1,1,1,1,
1,1,1,1,1,1,1,1,1,1,1,4),(0.0323453817713401,0.0983189520624214,0.14064060480402,
0.176193019733645,0.208307484243854,0.23948443235858,0.271287112904486,
0.28220667781497,0.293329328714142,0.304676551002397,0.319437818234531,
0.350137192454192,0.38765864687273,0.432002181900136,0.483167797782405,
0.541155494678712,0.605965272697963,0.67759713191795,0.75605107239617,0.841327094176323,
1.),.UNSPECIFIED.);
#236=B_SPLINE_CURVE_WITH_KNOTS('',3,(#9232,#9233,#9234,#9235,#9236,#9237,
#9238,#9239,#9240,#9241,#9242,#9243,#9244,#9245,#9246,#9247,#9248,#9249,
#9250,#9251,#9252,#9253,#9254),.UNSPECIFIED.,.F.,.F.,(4,1,1,1,1,1,1,1,1,
1,1,1,1,1,1,1,1,1,1,1,4),(0.,0.158672905823676,0.243948927603829,0.322402868082049,
0.394034727302036,0.458844505321287,0.516832202217594,0.567997818099863,
0.612341353127269,0.649862807545807,0.680562181765468,0.695323448997602,
0.706670671285856,0.717793322185029,0.728712887095513,0.760515567641419,
0.791692515756145,0.823806980266354,0.859359395195979,0.901681047937578,
0.967654618228659),.UNSPECIFIED.);
#237=B_SPLINE_CURVE_WITH_KNOTS('',3,(#9258,#9259,#9260,#9261,#9262,#9263,
#9264,#9265,#9266,#9267,#9268,#9269,#9270,#9271,#9272,#9273,#9274,#9275,
#9276,#9277,#9278,#9279,#9280),.UNSPECIFIED.,.F.,.F.,(4,1,1,1,1,1,1,1,1,
1,1,1,1,1,1,1,1,1,1,1,4),(0.0323453817713401,0.0983189520624214,0.14064060480402,
0.176193019733645,0.208307484243854,0.23948443235858,0.271287112904486,
0.28220667781497,0.293329328714142,0.304676551002397,0.319437818234531,
0.350137192454192,0.38765864687273,0.432002181900136,0.483167797782405,
0.541155494678712,0.605965272697963,0.67759713191795,0.75605107239617,0.841327094176323,
1.),.UNSPECIFIED.);
#238=B_SPLINE_CURVE_WITH_KNOTS('',3,(#9284,#9285,#9286,#9287,#9288,#9289,
#9290,#9291,#9292,#9293,#9294,#9295,#9296,#9297,#9298,#9299,#9300,#9301,
#9302,#9303,#9304,#9305,#9306),.UNSPECIFIED.,.F.,.F.,(4,1,1,1,1,1,1,1,1,
1,1,1,1,1,1,1,1,1,1,1,4),(0.,0.158672905823676,0.243948927603829,0.322402868082049,
0.394034727302036,0.458844505321287,0.516832202217594,0.567997818099863,
0.612341353127269,0.649862807545807,0.680562181765468,0.695323448997602,
0.706670671285856,0.717793322185029,0.728712887095513,0.760515567641419,
0.791692515756145,0.823806980266354,0.859359395195979,0.901681047937578,
0.967654618228659),.UNSPECIFIED.);
#239=B_SPLINE_CURVE_WITH_KNOTS('',3,(#9310,#9311,#9312,#9313,#9314,#9315,
#9316,#9317,#9318,#9319,#9320,#9321,#9322,#9323,#9324,#9325,#9326,#9327,
#9328,#9329,#9330,#9331,#9332),.UNSPECIFIED.,.F.,.F.,(4,1,1,1,1,1,1,1,1,
1,1,1,1,1,1,1,1,1,1,1,4),(0.0323453817713401,0.0983189520624214,0.14064060480402,
0.176193019733645,0.208307484243854,0.23948443235858,0.271287112904486,
0.28220667781497,0.293329328714142,0.304676551002397,0.319437818234531,
0.350137192454192,0.38765864687273,0.432002181900136,0.483167797782405,
0.541155494678712,0.605965272697963,0.67759713191795,0.75605107239617,0.841327094176323,
1.),.UNSPECIFIED.);
#240=B_SPLINE_CURVE_WITH_KNOTS('',3,(#9336,#9337,#9338,#9339,#9340,#9341,
#9342,#9343,#9344,#9345,#9346,#9347,#9348,#9349,#9350,#9351,#9352,#9353,
#9354,#9355,#9356,#9357,#9358),.UNSPECIFIED.,.F.,.F.,(4,1,1,1,1,1,1,1,1,
1,1,1,1,1,1,1,1,1,1,1,4),(0.,0.158672905823676,0.243948927603829,0.322402868082049,
0.394034727302036,0.458844505321287,0.516832202217594,0.567997818099863,
0.612341353127269,0.649862807545807,0.680562181765468,0.695323448997602,
0.706670671285856,0.717793322185029,0.728712887095513,0.760515567641419,
0.791692515756145,0.823806980266354,0.859359395195979,0.901681047937578,
0.967654618228659),.UNSPECIFIED.);
#241=B_SPLINE_CURVE_WITH_KNOTS('',3,(#9362,#9363,#9364,#9365,#9366,#9367,
#9368,#9369,#9370,#9371,#9372,#9373,#9374,#9375,#9376,#9377,#9378,#9379,
#9380,#9381,#9382,#9383,#9384),.UNSPECIFIED.,.F.,.F.,(4,1,1,1,1,1,1,1,1,
1,1,1,1,1,1,1,1,1,1,1,4),(0.0323453817713401,0.0983189520624214,0.14064060480402,
0.176193019733645,0.208307484243854,0.23948443235858,0.271287112904486,
0.28220667781497,0.293329328714142,0.304676551002397,0.319437818234531,
0.350137192454192,0.38765864687273,0.432002181900136,0.483167797782405,
0.541155494678712,0.605965272697963,0.67759713191795,0.75605107239617,0.841327094176323,
1.),.UNSPECIFIED.);
#242=B_SPLINE_CURVE_WITH_KNOTS('',3,(#9388,#9389,#9390,#9391,#9392,#9393,
#9394,#9395,#9396,#9397,#9398,#9399,#9400,#9401,#9402,#9403,#9404,#9405,
#9406,#9407,#9408,#9409,#9410),.UNSPECIFIED.,.F.,.F.,(4,1,1,1,1,1,1,1,1,
1,1,1,1,1,1,1,1,1,1,1,4),(0.,0.158672905823676,0.243948927603829,0.322402868082049,
0.394034727302036,0.458844505321287,0.516832202217594,0.567997818099863,
0.612341353127269,0.649862807545807,0.680562181765468,0.695323448997602,
0.706670671285856,0.717793322185029,0.728712887095513,0.760515567641419,
0.791692515756145,0.823806980266354,0.859359395195979,0.901681047937578,
0.967654618228659),.UNSPECIFIED.);
#243=B_SPLINE_CURVE_WITH_KNOTS('',3,(#9414,#9415,#9416,#9417,#9418,#9419,
#9420,#9421,#9422,#9423,#9424,#9425,#9426,#9427,#9428,#9429,#9430,#9431,
#9432,#9433,#9434,#9435,#9436),.UNSPECIFIED.,.F.,.F.,(4,1,1,1,1,1,1,1,1,
1,1,1,1,1,1,1,1,1,1,1,4),(0.0323453817713401,0.0983189520624214,0.14064060480402,
0.176193019733645,0.208307484243854,0.23948443235858,0.271287112904486,
0.28220667781497,0.293329328714142,0.304676551002397,0.319437818234531,
0.350137192454192,0.38765864687273,0.432002181900136,0.483167797782405,
0.541155494678712,0.605965272697963,0.67759713191795,0.75605107239617,0.841327094176323,
1.),.UNSPECIFIED.);
#244=B_SPLINE_CURVE_WITH_KNOTS('',3,(#9440,#9441,#9442,#9443,#9444,#9445,
#9446,#9447,#9448,#9449,#9450,#9451,#9452,#9453,#9454,#9455,#9456,#9457,
#9458,#9459,#9460,#9461,#9462),.UNSPECIFIED.,.F.,.F.,(4,1,1,1,1,1,1,1,1,
1,1,1,1,1,1,1,1,1,1,1,4),(0.,0.158672905823676,0.243948927603829,0.322402868082049,
0.394034727302036,0.458844505321287,0.516832202217594,0.567997818099863,
0.612341353127269,0.649862807545807,0.680562181765468,0.695323448997602,
0.706670671285856,0.717793322185029,0.728712887095513,0.760515567641419,
0.791692515756145,0.823806980266354,0.859359395195979,0.901681047937578,
0.967654618228659),.UNSPECIFIED.);
#245=B_SPLINE_CURVE_WITH_KNOTS('',3,(#9466,#9467,#9468,#9469,#9470,#9471,
#9472,#9473,#9474,#9475,#9476,#9477,#9478,#9479,#9480,#9481,#9482,#9483,
#9484,#9485,#9486,#9487,#9488),.UNSPECIFIED.,.F.,.F.,(4,1,1,1,1,1,1,1,1,
1,1,1,1,1,1,1,1,1,1,1,4),(0.0323453817713401,0.0983189520624214,0.14064060480402,
0.176193019733645,0.208307484243854,0.23948443235858,0.271287112904486,
0.28220667781497,0.293329328714142,0.304676551002397,0.319437818234531,
0.350137192454192,0.38765864687273,0.432002181900136,0.483167797782405,
0.541155494678712,0.605965272697963,0.67759713191795,0.75605107239617,0.841327094176323,
1.),.UNSPECIFIED.);
#246=B_SPLINE_CURVE_WITH_KNOTS('',3,(#9492,#9493,#9494,#9495,#9496,#9497,
#9498,#9499,#9500,#9501,#9502,#9503,#9504,#9505,#9506,#9507,#9508,#9509,
#9510,#9511,#9512,#9513,#9514),.UNSPECIFIED.,.F.,.F.,(4,1,1,1,1,1,1,1,1,
1,1,1,1,1,1,1,1,1,1,1,4),(0.,0.158672905823676,0.243948927603829,0.322402868082049,
0.394034727302036,0.458844505321287,0.516832202217594,0.567997818099863,
0.612341353127269,0.649862807545807,0.680562181765468,0.695323448997602,
0.706670671285856,0.717793322185029,0.728712887095513,0.760515567641419,
0.791692515756145,0.823806980266354,0.859359395195979,0.901681047937578,
0.967654618228659),.UNSPECIFIED.);
#247=B_SPLINE_CURVE_WITH_KNOTS('',3,(#9519,#9520,#9521,#9522,#9523,#9524,
#9525,#9526,#9527,#9528,#9529,#9530,#9531,#9532,#9533,#9534,#9535,#9536,
#9537,#9538,#9539,#9540,#9541),.UNSPECIFIED.,.F.,.F.,(4,1,1,1,1,1,1,1,1,
1,1,1,1,1,1,1,1,1,1,1,4),(0.0323453817713401,0.0983189520624214,0.14064060480402,
0.176193019733645,0.208307484243854,0.23948443235858,0.271287112904486,
0.28220667781497,0.293329328714142,0.304676551002397,0.319437818234531,
0.350137192454192,0.38765864687273,0.432002181900136,0.483167797782405,
0.541155494678712,0.605965272697963,0.67759713191795,0.75605107239617,0.841327094176323,
1.),.UNSPECIFIED.);
#248=B_SPLINE_CURVE_WITH_KNOTS('',3,(#9545,#9546,#9547,#9548,#9549,#9550,
#9551,#9552,#9553,#9554,#9555,#9556,#9557,#9558,#9559,#9560,#9561,#9562,
#9563,#9564,#9565,#9566,#9567),.UNSPECIFIED.,.F.,.F.,(4,1,1,1,1,1,1,1,1,
1,1,1,1,1,1,1,1,1,1,1,4),(0.,0.158672905823676,0.243948927603829,0.322402868082049,
0.394034727302036,0.458844505321287,0.516832202217594,0.567997818099863,
0.612341353127269,0.649862807545807,0.680562181765468,0.695323448997602,
0.706670671285856,0.717793322185029,0.728712887095513,0.760515567641419,
0.791692515756145,0.823806980266354,0.859359395195979,0.901681047937578,
0.967654618228659),.UNSPECIFIED.);
#249=B_SPLINE_CURVE_WITH_KNOTS('',3,(#9571,#9572,#9573,#9574,#9575,#9576,
#9577,#9578,#9579,#9580,#9581,#9582,#9583,#9584,#9585,#9586,#9587,#9588,
#9589,#9590,#9591,#9592,#9593),.UNSPECIFIED.,.F.,.F.,(4,1,1,1,1,1,1,1,1,
1,1,1,1,1,1,1,1,1,1,1,4),(0.0323453817713401,0.0983189520624214,0.14064060480402,
0.176193019733645,0.208307484243854,0.23948443235858,0.271287112904486,
0.28220667781497,0.293329328714142,0.304676551002397,0.319437818234531,
0.350137192454192,0.38765864687273,0.432002181900136,0.483167797782405,
0.541155494678712,0.605965272697963,0.67759713191795,0.75605107239617,0.841327094176323,
1.),.UNSPECIFIED.);
#250=B_SPLINE_CURVE_WITH_KNOTS('',3,(#9597,#9598,#9599,#9600,#9601,#9602,
#9603,#9604,#9605,#9606,#9607,#9608,#9609,#9610,#9611,#9612,#9613,#9614,
#9615,#9616,#9617,#9618,#9619),.UNSPECIFIED.,.F.,.F.,(4,1,1,1,1,1,1,1,1,
1,1,1,1,1,1,1,1,1,1,1,4),(0.,0.158672905823676,0.243948927603829,0.322402868082049,
0.394034727302036,0.458844505321287,0.516832202217594,0.567997818099863,
0.612341353127269,0.649862807545807,0.680562181765468,0.695323448997602,
0.706670671285856,0.717793322185029,0.728712887095513,0.760515567641419,
0.791692515756145,0.823806980266354,0.859359395195979,0.901681047937578,
0.967654618228659),.UNSPECIFIED.);
#251=B_SPLINE_CURVE_WITH_KNOTS('',3,(#9623,#9624,#9625,#9626,#9627,#9628,
#9629,#9630,#9631,#9632,#9633,#9634,#9635,#9636,#9637,#9638,#9639,#9640,
#9641,#9642,#9643,#9644,#9645),.UNSPECIFIED.,.F.,.F.,(4,1,1,1,1,1,1,1,1,
1,1,1,1,1,1,1,1,1,1,1,4),(0.0323453817713401,0.0983189520624214,0.14064060480402,
0.176193019733645,0.208307484243854,0.23948443235858,0.271287112904486,
0.28220667781497,0.293329328714142,0.304676551002397,0.319437818234531,
0.350137192454192,0.38765864687273,0.432002181900136,0.483167797782405,
0.541155494678712,0.605965272697963,0.67759713191795,0.75605107239617,0.841327094176323,
1.),.UNSPECIFIED.);
#252=B_SPLINE_CURVE_WITH_KNOTS('',3,(#9649,#9650,#9651,#9652,#9653,#9654,
#9655,#9656,#9657,#9658,#9659,#9660,#9661,#9662,#9663,#9664,#9665,#9666,
#9667,#9668,#9669,#9670,#9671),.UNSPECIFIED.,.F.,.F.,(4,1,1,1,1,1,1,1,1,
1,1,1,1,1,1,1,1,1,1,1,4),(0.,0.158672905823676,0.243948927603829,0.322402868082049,
0.394034727302036,0.458844505321287,0.516832202217594,0.567997818099863,
0.612341353127269,0.649862807545807,0.680562181765468,0.695323448997602,
0.706670671285856,0.717793322185029,0.728712887095513,0.760515567641419,
0.791692515756145,0.823806980266354,0.859359395195979,0.901681047937578,
0.967654618228659),.UNSPECIFIED.);
#253=B_SPLINE_CURVE_WITH_KNOTS('',3,(#9675,#9676,#9677,#9678,#9679,#9680,
#9681,#9682,#9683,#9684,#9685,#9686,#9687,#9688,#9689,#9690,#9691,#9692,
#9693,#9694,#9695,#9696,#9697),.UNSPECIFIED.,.F.,.F.,(4,1,1,1,1,1,1,1,1,
1,1,1,1,1,1,1,1,1,1,1,4),(0.0323453817713401,0.0983189520624214,0.14064060480402,
0.176193019733645,0.208307484243854,0.23948443235858,0.271287112904486,
0.28220667781497,0.293329328714142,0.304676551002397,0.319437818234531,
0.350137192454192,0.38765864687273,0.432002181900136,0.483167797782405,
0.541155494678712,0.605965272697963,0.67759713191795,0.75605107239617,0.841327094176323,
1.),.UNSPECIFIED.);
#254=B_SPLINE_CURVE_WITH_KNOTS('',3,(#9701,#9702,#9703,#9704,#9705,#9706,
#9707,#9708,#9709,#9710,#9711,#9712,#9713,#9714,#9715,#9716,#9717,#9718,
#9719,#9720,#9721,#9722,#9723),.UNSPECIFIED.,.F.,.F.,(4,1,1,1,1,1,1,1,1,
1,1,1,1,1,1,1,1,1,1,1,4),(0.,0.158672905823676,0.243948927603829,0.322402868082049,
0.394034727302036,0.458844505321287,0.516832202217594,0.567997818099863,
0.612341353127269,0.649862807545807,0.680562181765468,0.695323448997602,
0.706670671285856,0.717793322185029,0.728712887095513,0.760515567641419,
0.791692515756145,0.823806980266354,0.859359395195979,0.901681047937578,
0.967654618228659),.UNSPECIFIED.);
#255=B_SPLINE_CURVE_WITH_KNOTS('',3,(#9727,#9728,#9729,#9730,#9731,#9732,
#9733,#9734,#9735,#9736,#9737,#9738,#9739,#9740,#9741,#9742,#9743,#9744,
#9745,#9746,#9747,#9748,#9749),.UNSPECIFIED.,.F.,.F.,(4,1,1,1,1,1,1,1,1,
1,1,1,1,1,1,1,1,1,1,1,4),(0.0323453817713401,0.0983189520624214,0.14064060480402,
0.176193019733645,0.208307484243854,0.23948443235858,0.271287112904486,
0.28220667781497,0.293329328714142,0.304676551002397,0.319437818234531,
0.350137192454192,0.38765864687273,0.432002181900136,0.483167797782405,
0.541155494678712,0.605965272697963,0.67759713191795,0.75605107239617,0.841327094176323,
1.),.UNSPECIFIED.);
#256=B_SPLINE_CURVE_WITH_KNOTS('',3,(#9753,#9754,#9755,#9756,#9757,#9758,
#9759,#9760,#9761,#9762,#9763,#9764,#9765,#9766,#9767,#9768,#9769,#9770,
#9771,#9772,#9773,#9774,#9775),.UNSPECIFIED.,.F.,.F.,(4,1,1,1,1,1,1,1,1,
1,1,1,1,1,1,1,1,1,1,1,4),(0.,0.158672905823676,0.243948927603829,0.322402868082049,
0.394034727302036,0.458844505321287,0.516832202217594,0.567997818099863,
0.612341353127269,0.649862807545807,0.680562181765468,0.695323448997602,
0.706670671285856,0.717793322185029,0.728712887095513,0.760515567641419,
0.791692515756145,0.823806980266354,0.859359395195979,0.901681047937578,
0.967654618228659),.UNSPECIFIED.);
#257=B_SPLINE_CURVE_WITH_KNOTS('',3,(#9779,#9780,#9781,#9782,#9783,#9784,
#9785,#9786,#9787,#9788,#9789,#9790,#9791,#9792,#9793,#9794,#9795,#9796,
#9797,#9798,#9799,#9800,#9801),.UNSPECIFIED.,.F.,.F.,(4,1,1,1,1,1,1,1,1,
1,1,1,1,1,1,1,1,1,1,1,4),(0.0323453817713401,0.0983189520624214,0.14064060480402,
0.176193019733645,0.208307484243854,0.23948443235858,0.271287112904486,
0.28220667781497,0.293329328714142,0.304676551002397,0.319437818234531,
0.350137192454192,0.38765864687273,0.432002181900136,0.483167797782405,
0.541155494678712,0.605965272697963,0.67759713191795,0.75605107239617,0.841327094176323,
1.),.UNSPECIFIED.);
#258=B_SPLINE_CURVE_WITH_KNOTS('',3,(#9805,#9806,#9807,#9808,#9809,#9810,
#9811,#9812,#9813,#9814,#9815,#9816,#9817,#9818,#9819,#9820,#9821,#9822,
#9823,#9824,#9825,#9826,#9827),.UNSPECIFIED.,.F.,.F.,(4,1,1,1,1,1,1,1,1,
1,1,1,1,1,1,1,1,1,1,1,4),(0.,0.158672905823676,0.243948927603829,0.322402868082049,
0.394034727302036,0.458844505321287,0.516832202217594,0.567997818099863,
0.612341353127269,0.649862807545807,0.680562181765468,0.695323448997602,
0.706670671285856,0.717793322185029,0.728712887095513,0.760515567641419,
0.791692515756145,0.823806980266354,0.859359395195979,0.901681047937578,
0.967654618228659),.UNSPECIFIED.);
#259=B_SPLINE_CURVE_WITH_KNOTS('',3,(#9831,#9832,#9833,#9834,#9835,#9836,
#9837,#9838,#9839,#9840,#9841,#9842,#9843,#9844,#9845,#9846,#9847,#9848,
#9849,#9850,#9851,#9852,#9853),.UNSPECIFIED.,.F.,.F.,(4,1,1,1,1,1,1,1,1,
1,1,1,1,1,1,1,1,1,1,1,4),(0.0323453817713401,0.0983189520624214,0.14064060480402,
0.176193019733645,0.208307484243854,0.23948443235858,0.271287112904486,
0.28220667781497,0.293329328714142,0.304676551002397,0.319437818234531,
0.350137192454192,0.38765864687273,0.432002181900136,0.483167797782405,
0.541155494678712,0.605965272697963,0.67759713191795,0.75605107239617,0.841327094176323,
1.),.UNSPECIFIED.);
#260=B_SPLINE_CURVE_WITH_KNOTS('',3,(#9857,#9858,#9859,#9860,#9861,#9862,
#9863,#9864,#9865,#9866,#9867,#9868,#9869,#9870,#9871,#9872,#9873,#9874,
#9875,#9876,#9877,#9878,#9879),.UNSPECIFIED.,.F.,.F.,(4,1,1,1,1,1,1,1,1,
1,1,1,1,1,1,1,1,1,1,1,4),(0.,0.158672905823676,0.243948927603829,0.322402868082049,
0.394034727302036,0.458844505321287,0.516832202217594,0.567997818099863,
0.612341353127269,0.649862807545807,0.680562181765468,0.695323448997602,
0.706670671285856,0.717793322185029,0.728712887095513,0.760515567641419,
0.791692515756145,0.823806980266354,0.859359395195979,0.901681047937578,
0.967654618228659),.UNSPECIFIED.);
#261=B_SPLINE_CURVE_WITH_KNOTS('',3,(#9883,#9884,#9885,#9886,#9887,#9888,
#9889,#9890,#9891,#9892,#9893,#9894,#9895,#9896,#9897,#9898,#9899,#9900,
#9901,#9902,#9903,#9904,#9905),.UNSPECIFIED.,.F.,.F.,(4,1,1,1,1,1,1,1,1,
1,1,1,1,1,1,1,1,1,1,1,4),(0.0323453817713401,0.0983189520624214,0.14064060480402,
0.176193019733645,0.208307484243854,0.23948443235858,0.271287112904486,
0.28220667781497,0.293329328714142,0.304676551002397,0.319437818234531,
0.350137192454192,0.38765864687273,0.432002181900136,0.483167797782405,
0.541155494678712,0.605965272697963,0.67759713191795,0.75605107239617,0.841327094176323,
1.),.UNSPECIFIED.);
#262=B_SPLINE_CURVE_WITH_KNOTS('',3,(#9909,#9910,#9911,#9912,#9913,#9914,
#9915,#9916,#9917,#9918,#9919,#9920,#9921,#9922,#9923,#9924,#9925,#9926,
#9927,#9928,#9929,#9930,#9931),.UNSPECIFIED.,.F.,.F.,(4,1,1,1,1,1,1,1,1,
1,1,1,1,1,1,1,1,1,1,1,4),(0.,0.158672905823676,0.243948927603829,0.322402868082049,
0.394034727302036,0.458844505321287,0.516832202217594,0.567997818099863,
0.612341353127269,0.649862807545807,0.680562181765468,0.695323448997602,
0.706670671285856,0.717793322185029,0.728712887095513,0.760515567641419,
0.791692515756145,0.823806980266354,0.859359395195979,0.901681047937578,
0.967654618228659),.UNSPECIFIED.);
#263=B_SPLINE_CURVE_WITH_KNOTS('',3,(#9935,#9936,#9937,#9938,#9939,#9940,
#9941,#9942,#9943,#9944,#9945,#9946,#9947,#9948,#9949,#9950,#9951,#9952,
#9953,#9954,#9955,#9956,#9957),.UNSPECIFIED.,.F.,.F.,(4,1,1,1,1,1,1,1,1,
1,1,1,1,1,1,1,1,1,1,1,4),(0.0323453817713401,0.0983189520624214,0.14064060480402,
0.176193019733645,0.208307484243854,0.23948443235858,0.271287112904486,
0.28220667781497,0.293329328714142,0.304676551002397,0.319437818234531,
0.350137192454192,0.38765864687273,0.432002181900136,0.483167797782405,
0.541155494678712,0.605965272697963,0.67759713191795,0.75605107239617,0.841327094176323,
1.),.UNSPECIFIED.);
#264=B_SPLINE_CURVE_WITH_KNOTS('',3,(#9961,#9962,#9963,#9964,#9965,#9966,
#9967,#9968,#9969,#9970,#9971,#9972,#9973,#9974,#9975,#9976,#9977,#9978,
#9979,#9980,#9981,#9982,#9983),.UNSPECIFIED.,.F.,.F.,(4,1,1,1,1,1,1,1,1,
1,1,1,1,1,1,1,1,1,1,1,4),(0.,0.158672905823676,0.243948927603829,0.322402868082049,
0.394034727302036,0.458844505321287,0.516832202217594,0.567997818099863,
0.612341353127269,0.649862807545807,0.680562181765468,0.695323448997602,
0.706670671285856,0.717793322185029,0.728712887095513,0.760515567641419,
0.791692515756145,0.823806980266354,0.859359395195979,0.901681047937578,
0.967654618228659),.UNSPECIFIED.);
#265=B_SPLINE_CURVE_WITH_KNOTS('',3,(#9987,#9988,#9989,#9990,#9991,#9992,
#9993,#9994,#9995,#9996,#9997,#9998,#9999,#10000,#10001,#10002,#10003,#10004,
#10005,#10006,#10007,#10008,#10009),.UNSPECIFIED.,.F.,.F.,(4,1,1,1,1,1,
1,1,1,1,1,1,1,1,1,1,1,1,1,1,4),(0.0323453817713401,0.0983189520624214,0.14064060480402,
0.176193019733645,0.208307484243854,0.23948443235858,0.271287112904486,
0.28220667781497,0.293329328714142,0.304676551002397,0.319437818234531,
0.350137192454192,0.38765864687273,0.432002181900136,0.483167797782405,
0.541155494678712,0.605965272697963,0.67759713191795,0.75605107239617,0.841327094176323,
1.),.UNSPECIFIED.);
#266=B_SPLINE_CURVE_WITH_KNOTS('',3,(#10013,#10014,#10015,#10016,#10017,
#10018,#10019,#10020,#10021,#10022,#10023,#10024,#10025,#10026,#10027,#10028,
#10029,#10030,#10031,#10032,#10033,#10034,#10035),.UNSPECIFIED.,.F.,.F.,
(4,1,1,1,1,1,1,1,1,1,1,1,1,1,1,1,1,1,1,1,4),(0.,0.158672905823676,0.243948927603829,
0.322402868082049,0.394034727302036,0.458844505321287,0.516832202217594,
0.567997818099863,0.612341353127269,0.649862807545807,0.680562181765468,
0.695323448997602,0.706670671285856,0.717793322185029,0.728712887095513,
0.760515567641419,0.791692515756145,0.823806980266354,0.859359395195979,
0.901681047937578,0.967654618228659),.UNSPECIFIED.);
#267=B_SPLINE_CURVE_WITH_KNOTS('',3,(#10039,#10040,#10041,#10042,#10043,
#10044,#10045,#10046,#10047,#10048,#10049,#10050,#10051,#10052,#10053,#10054,
#10055,#10056,#10057,#10058,#10059,#10060,#10061),.UNSPECIFIED.,.F.,.F.,
(4,1,1,1,1,1,1,1,1,1,1,1,1,1,1,1,1,1,1,1,4),(0.0323453817713401,0.0983189520624214,
0.14064060480402,0.176193019733645,0.208307484243854,0.23948443235858,0.271287112904486,
0.28220667781497,0.293329328714142,0.304676551002397,0.319437818234531,
0.350137192454192,0.38765864687273,0.432002181900136,0.483167797782405,
0.541155494678712,0.605965272697963,0.67759713191795,0.75605107239617,0.841327094176323,
1.),.UNSPECIFIED.);
#268=B_SPLINE_CURVE_WITH_KNOTS('',3,(#10065,#10066,#10067,#10068,#10069,
#10070,#10071,#10072,#10073,#10074,#10075,#10076,#10077,#10078,#10079,#10080,
#10081,#10082,#10083,#10084,#10085,#10086,#10087),.UNSPECIFIED.,.F.,.F.,
(4,1,1,1,1,1,1,1,1,1,1,1,1,1,1,1,1,1,1,1,4),(0.,0.158672905823676,0.243948927603829,
0.322402868082049,0.394034727302036,0.458844505321287,0.516832202217594,
0.567997818099863,0.612341353127269,0.649862807545807,0.680562181765468,
0.695323448997602,0.706670671285856,0.717793322185029,0.728712887095513,
0.760515567641419,0.791692515756145,0.823806980266354,0.859359395195979,
0.901681047937578,0.967654618228659),.UNSPECIFIED.);
#269=B_SPLINE_CURVE_WITH_KNOTS('',3,(#10090,#10091,#10092,#10093,#10094,
#10095,#10096,#10097,#10098,#10099,#10100,#10101,#10102,#10103,#10104,#10105,
#10106,#10107,#10108,#10109,#10110,#10111,#10112),.UNSPECIFIED.,.F.,.F.,
(4,1,1,1,1,1,1,1,1,1,1,1,1,1,1,1,1,1,1,1,4),(0.0323453817713401,0.0983189520624214,
0.14064060480402,0.176193019733645,0.208307484243854,0.23948443235858,0.271287112904486,
0.28220667781497,0.293329328714142,0.304676551002397,0.319437818234531,
0.350137192454192,0.38765864687273,0.432002181900136,0.483167797782405,
0.541155494678712,0.605965272697963,0.67759713191795,0.75605107239617,0.841327094176323,
1.),.UNSPECIFIED.);
#270=B_SPLINE_CURVE_WITH_KNOTS('',3,(#10114,#10115,#10116,#10117,#10118,
#10119,#10120,#10121,#10122,#10123,#10124,#10125,#10126,#10127,#10128,#10129,
#10130,#10131,#10132,#10133,#10134,#10135,#10136),.UNSPECIFIED.,.F.,.F.,
(4,1,1,1,1,1,1,1,1,1,1,1,1,1,1,1,1,1,1,1,4),(0.,0.158672905823676,0.243948927603829,
0.322402868082049,0.394034727302036,0.458844505321287,0.516832202217594,
0.567997818099863,0.612341353127269,0.649862807545807,0.680562181765468,
0.695323448997602,0.706670671285856,0.717793322185029,0.728712887095513,
0.760515567641419,0.791692515756145,0.823806980266354,0.859359395195979,
0.901681047937578,0.967654618228659),.UNSPECIFIED.);
#271=B_SPLINE_CURVE_WITH_KNOTS('',3,(#10140,#10141,#10142,#10143,#10144,
#10145,#10146,#10147,#10148,#10149,#10150,#10151,#10152,#10153,#10154,#10155,
#10156,#10157,#10158,#10159,#10160,#10161,#10162),.UNSPECIFIED.,.F.,.F.,
(4,1,1,1,1,1,1,1,1,1,1,1,1,1,1,1,1,1,1,1,4),(0.0323453817713401,0.0983189520624214,
0.14064060480402,0.176193019733645,0.208307484243854,0.23948443235858,0.271287112904486,
0.28220667781497,0.293329328714142,0.304676551002397,0.319437818234531,
0.350137192454192,0.38765864687273,0.432002181900136,0.483167797782405,
0.541155494678712,0.605965272697963,0.67759713191795,0.75605107239617,0.841327094176323,
1.),.UNSPECIFIED.);
#272=B_SPLINE_CURVE_WITH_KNOTS('',3,(#10166,#10167,#10168,#10169,#10170,
#10171,#10172,#10173,#10174,#10175,#10176,#10177,#10178,#10179,#10180,#10181,
#10182,#10183,#10184,#10185,#10186,#10187,#10188),.UNSPECIFIED.,.F.,.F.,
(4,1,1,1,1,1,1,1,1,1,1,1,1,1,1,1,1,1,1,1,4),(0.,0.158672905823676,0.243948927603829,
0.322402868082049,0.394034727302036,0.458844505321287,0.516832202217594,
0.567997818099863,0.612341353127269,0.649862807545807,0.680562181765468,
0.695323448997602,0.706670671285856,0.717793322185029,0.728712887095513,
0.760515567641419,0.791692515756145,0.823806980266354,0.859359395195979,
0.901681047937578,0.967654618228659),.UNSPECIFIED.);
#273=B_SPLINE_CURVE_WITH_KNOTS('',3,(#10192,#10193,#10194,#10195,#10196,
#10197,#10198,#10199,#10200,#10201,#10202,#10203,#10204,#10205,#10206,#10207,
#10208,#10209,#10210,#10211,#10212,#10213,#10214),.UNSPECIFIED.,.F.,.F.,
(4,1,1,1,1,1,1,1,1,1,1,1,1,1,1,1,1,1,1,1,4),(0.0323453817713401,0.0983189520624214,
0.14064060480402,0.176193019733645,0.208307484243854,0.23948443235858,0.271287112904486,
0.28220667781497,0.293329328714142,0.304676551002397,0.319437818234531,
0.350137192454192,0.38765864687273,0.432002181900136,0.483167797782405,
0.541155494678712,0.605965272697963,0.67759713191795,0.75605107239617,0.841327094176323,
1.),.UNSPECIFIED.);
#274=B_SPLINE_CURVE_WITH_KNOTS('',3,(#10218,#10219,#10220,#10221,#10222,
#10223,#10224,#10225,#10226,#10227,#10228,#10229,#10230,#10231,#10232,#10233,
#10234,#10235,#10236,#10237,#10238,#10239,#10240),.UNSPECIFIED.,.F.,.F.,
(4,1,1,1,1,1,1,1,1,1,1,1,1,1,1,1,1,1,1,1,4),(0.,0.158672905823676,0.243948927603829,
0.322402868082049,0.394034727302036,0.458844505321287,0.516832202217594,
0.567997818099863,0.612341353127269,0.649862807545807,0.680562181765468,
0.695323448997602,0.706670671285856,0.717793322185029,0.728712887095513,
0.760515567641419,0.791692515756145,0.823806980266354,0.859359395195979,
0.901681047937578,0.967654618228659),.UNSPECIFIED.);
#275=B_SPLINE_CURVE_WITH_KNOTS('',3,(#10244,#10245,#10246,#10247,#10248,
#10249,#10250,#10251,#10252,#10253,#10254,#10255,#10256,#10257,#10258,#10259,
#10260,#10261,#10262,#10263,#10264,#10265,#10266),.UNSPECIFIED.,.F.,.F.,
(4,1,1,1,1,1,1,1,1,1,1,1,1,1,1,1,1,1,1,1,4),(0.0323453817713401,0.0983189520624214,
0.14064060480402,0.176193019733645,0.208307484243854,0.23948443235858,0.271287112904486,
0.28220667781497,0.293329328714142,0.304676551002397,0.319437818234531,
0.350137192454192,0.38765864687273,0.432002181900136,0.483167797782405,
0.541155494678712,0.605965272697963,0.67759713191795,0.75605107239617,0.841327094176323,
1.),.UNSPECIFIED.);
#276=B_SPLINE_CURVE_WITH_KNOTS('',3,(#10270,#10271,#10272,#10273,#10274,
#10275,#10276,#10277,#10278,#10279,#10280,#10281,#10282,#10283,#10284,#10285,
#10286,#10287,#10288,#10289,#10290,#10291,#10292),.UNSPECIFIED.,.F.,.F.,
(4,1,1,1,1,1,1,1,1,1,1,1,1,1,1,1,1,1,1,1,4),(0.,0.158672905823676,0.243948927603829,
0.322402868082049,0.394034727302036,0.458844505321287,0.516832202217594,
0.567997818099863,0.612341353127269,0.649862807545807,0.680562181765468,
0.695323448997602,0.706670671285856,0.717793322185029,0.728712887095513,
0.760515567641419,0.791692515756145,0.823806980266354,0.859359395195979,
0.901681047937578,0.967654618228659),.UNSPECIFIED.);
#277=B_SPLINE_CURVE_WITH_KNOTS('',3,(#10296,#10297,#10298,#10299,#10300,
#10301,#10302,#10303,#10304,#10305,#10306,#10307,#10308,#10309,#10310,#10311,
#10312,#10313,#10314,#10315,#10316,#10317,#10318),.UNSPECIFIED.,.F.,.F.,
(4,1,1,1,1,1,1,1,1,1,1,1,1,1,1,1,1,1,1,1,4),(0.0323453817713401,0.0983189520624214,
0.14064060480402,0.176193019733645,0.208307484243854,0.23948443235858,0.271287112904486,
0.28220667781497,0.293329328714142,0.304676551002397,0.319437818234531,
0.350137192454192,0.38765864687273,0.432002181900136,0.483167797782405,
0.541155494678712,0.605965272697963,0.67759713191795,0.75605107239617,0.841327094176323,
1.),.UNSPECIFIED.);
#278=B_SPLINE_CURVE_WITH_KNOTS('',3,(#10322,#10323,#10324,#10325,#10326,
#10327,#10328,#10329,#10330,#10331,#10332,#10333,#10334,#10335,#10336,#10337,
#10338,#10339,#10340,#10341,#10342,#10343,#10344),.UNSPECIFIED.,.F.,.F.,
(4,1,1,1,1,1,1,1,1,1,1,1,1,1,1,1,1,1,1,1,4),(0.,0.158672905823676,0.243948927603829,
0.322402868082049,0.394034727302036,0.458844505321287,0.516832202217594,
0.567997818099863,0.612341353127269,0.649862807545807,0.680562181765468,
0.695323448997602,0.706670671285856,0.717793322185029,0.728712887095513,
0.760515567641419,0.791692515756145,0.823806980266354,0.859359395195979,
0.901681047937578,0.967654618228659),.UNSPECIFIED.);
#279=B_SPLINE_CURVE_WITH_KNOTS('',3,(#10348,#10349,#10350,#10351,#10352,
#10353,#10354,#10355,#10356,#10357,#10358,#10359,#10360,#10361,#10362,#10363,
#10364,#10365,#10366,#10367,#10368,#10369,#10370),.UNSPECIFIED.,.F.,.F.,
(4,1,1,1,1,1,1,1,1,1,1,1,1,1,1,1,1,1,1,1,4),(0.0323453817713401,0.0983189520624214,
0.14064060480402,0.176193019733645,0.208307484243854,0.23948443235858,0.271287112904486,
0.28220667781497,0.293329328714142,0.304676551002397,0.319437818234531,
0.350137192454192,0.38765864687273,0.432002181900136,0.483167797782405,
0.541155494678712,0.605965272697963,0.67759713191795,0.75605107239617,0.841327094176323,
1.),.UNSPECIFIED.);
#280=B_SPLINE_CURVE_WITH_KNOTS('',3,(#10374,#10375,#10376,#10377,#10378,
#10379,#10380,#10381,#10382,#10383,#10384,#10385,#10386,#10387,#10388,#10389,
#10390,#10391,#10392,#10393,#10394,#10395,#10396),.UNSPECIFIED.,.F.,.F.,
(4,1,1,1,1,1,1,1,1,1,1,1,1,1,1,1,1,1,1,1,4),(0.,0.158672905823676,0.243948927603829,
0.322402868082049,0.394034727302036,0.458844505321287,0.516832202217594,
0.567997818099863,0.612341353127269,0.649862807545807,0.680562181765468,
0.695323448997602,0.706670671285856,0.717793322185029,0.728712887095513,
0.760515567641419,0.791692515756145,0.823806980266354,0.859359395195979,
0.901681047937578,0.967654618228659),.UNSPECIFIED.);
#281=B_SPLINE_CURVE_WITH_KNOTS('',3,(#10400,#10401,#10402,#10403,#10404,
#10405,#10406,#10407,#10408,#10409,#10410,#10411,#10412,#10413,#10414,#10415,
#10416,#10417,#10418,#10419,#10420,#10421,#10422),.UNSPECIFIED.,.F.,.F.,
(4,1,1,1,1,1,1,1,1,1,1,1,1,1,1,1,1,1,1,1,4),(0.0323453817713401,0.0983189520624214,
0.14064060480402,0.176193019733645,0.208307484243854,0.23948443235858,0.271287112904486,
0.28220667781497,0.293329328714142,0.304676551002397,0.319437818234531,
0.350137192454192,0.38765864687273,0.432002181900136,0.483167797782405,
0.541155494678712,0.605965272697963,0.67759713191795,0.75605107239617,0.841327094176323,
1.),.UNSPECIFIED.);
#282=B_SPLINE_CURVE_WITH_KNOTS('',3,(#10426,#10427,#10428,#10429,#10430,
#10431,#10432,#10433,#10434,#10435,#10436,#10437,#10438,#10439,#10440,#10441,
#10442,#10443,#10444,#10445,#10446,#10447,#10448),.UNSPECIFIED.,.F.,.F.,
(4,1,1,1,1,1,1,1,1,1,1,1,1,1,1,1,1,1,1,1,4),(0.,0.158672905823676,0.243948927603829,
0.322402868082049,0.394034727302036,0.458844505321287,0.516832202217594,
0.567997818099863,0.612341353127269,0.649862807545807,0.680562181765468,
0.695323448997602,0.706670671285856,0.717793322185029,0.728712887095513,
0.760515567641419,0.791692515756145,0.823806980266354,0.859359395195979,
0.901681047937578,0.967654618228659),.UNSPECIFIED.);
#283=B_SPLINE_CURVE_WITH_KNOTS('',3,(#10452,#10453,#10454,#10455,#10456,
#10457,#10458,#10459,#10460,#10461,#10462,#10463,#10464,#10465,#10466,#10467,
#10468,#10469,#10470,#10471,#10472,#10473,#10474),.UNSPECIFIED.,.F.,.F.,
(4,1,1,1,1,1,1,1,1,1,1,1,1,1,1,1,1,1,1,1,4),(0.0323453817713401,0.0983189520624214,
0.14064060480402,0.176193019733645,0.208307484243854,0.23948443235858,0.271287112904486,
0.28220667781497,0.293329328714142,0.304676551002397,0.319437818234531,
0.350137192454192,0.38765864687273,0.432002181900136,0.483167797782405,
0.541155494678712,0.605965272697963,0.67759713191795,0.75605107239617,0.841327094176323,
1.),.UNSPECIFIED.);
#284=B_SPLINE_CURVE_WITH_KNOTS('',3,(#10478,#10479,#10480,#10481,#10482,
#10483,#10484,#10485,#10486,#10487,#10488,#10489,#10490,#10491,#10492,#10493,
#10494,#10495,#10496,#10497,#10498,#10499,#10500),.UNSPECIFIED.,.F.,.F.,
(4,1,1,1,1,1,1,1,1,1,1,1,1,1,1,1,1,1,1,1,4),(0.,0.158672905823676,0.243948927603829,
0.322402868082049,0.394034727302036,0.458844505321287,0.516832202217594,
0.567997818099863,0.612341353127269,0.649862807545807,0.680562181765468,
0.695323448997602,0.706670671285856,0.717793322185029,0.728712887095513,
0.760515567641419,0.791692515756145,0.823806980266354,0.859359395195979,
0.901681047937578,0.967654618228659),.UNSPECIFIED.);
#285=B_SPLINE_CURVE_WITH_KNOTS('',3,(#10504,#10505,#10506,#10507,#10508,
#10509,#10510,#10511,#10512,#10513,#10514,#10515,#10516,#10517,#10518,#10519,
#10520,#10521,#10522,#10523,#10524,#10525,#10526),.UNSPECIFIED.,.F.,.F.,
(4,1,1,1,1,1,1,1,1,1,1,1,1,1,1,1,1,1,1,1,4),(0.0323453817713401,0.0983189520624214,
0.14064060480402,0.176193019733645,0.208307484243854,0.23948443235858,0.271287112904486,
0.28220667781497,0.293329328714142,0.304676551002397,0.319437818234531,
0.350137192454192,0.38765864687273,0.432002181900136,0.483167797782405,
0.541155494678712,0.605965272697963,0.67759713191795,0.75605107239617,0.841327094176323,
1.),.UNSPECIFIED.);
#286=B_SPLINE_CURVE_WITH_KNOTS('',3,(#10530,#10531,#10532,#10533,#10534,
#10535,#10536,#10537,#10538,#10539,#10540,#10541,#10542,#10543,#10544,#10545,
#10546,#10547,#10548,#10549,#10550,#10551,#10552),.UNSPECIFIED.,.F.,.F.,
(4,1,1,1,1,1,1,1,1,1,1,1,1,1,1,1,1,1,1,1,4),(0.,0.158672905823676,0.243948927603829,
0.322402868082049,0.394034727302036,0.458844505321287,0.516832202217594,
0.567997818099863,0.612341353127269,0.649862807545807,0.680562181765468,
0.695323448997602,0.706670671285856,0.717793322185029,0.728712887095513,
0.760515567641419,0.791692515756145,0.823806980266354,0.859359395195979,
0.901681047937578,0.967654618228659),.UNSPECIFIED.);
#287=SHAPE_REPRESENTATION_RELATIONSHIP('SRR','None',#13025,#295);
#288=SHAPE_REPRESENTATION_RELATIONSHIP('SRR','None',#13026,#296);
#289=SHAPE_REPRESENTATION_RELATIONSHIP('SRR','None',#13027,#297);
#290=SHAPE_REPRESENTATION_RELATIONSHIP('SRR','None',#13028,#298);
#291=SHAPE_REPRESENTATION_RELATIONSHIP('SRR','None',#13029,#299);
#292=SHAPE_REPRESENTATION_RELATIONSHIP('SRR','None',#13030,#300);
#293=SHAPE_REPRESENTATION_RELATIONSHIP('SRR','None',#13031,#301);
#294=SHAPE_REPRESENTATION_RELATIONSHIP('SRR','None',#13032,#302);
#295=ADVANCED_BREP_SHAPE_REPRESENTATION('',(#315,#316,#317,#318,#319),#12958);
#296=ADVANCED_BREP_SHAPE_REPRESENTATION('',(#320),#12959);
#297=ADVANCED_BREP_SHAPE_REPRESENTATION('',(#321),#12960);
#298=ADVANCED_BREP_SHAPE_REPRESENTATION('',(#322),#12961);
#299=ADVANCED_BREP_SHAPE_REPRESENTATION('',(#323),#12962);
#300=ADVANCED_BREP_SHAPE_REPRESENTATION('',(#324),#12963);
#301=ADVANCED_BREP_SHAPE_REPRESENTATION('',(#325),#12964);
#302=ADVANCED_BREP_SHAPE_REPRESENTATION('',(#326),#12965);
#303=STYLED_ITEM('',(#13074),#315);
#304=STYLED_ITEM('',(#13074),#316);
#305=STYLED_ITEM('',(#13074),#317);
#306=STYLED_ITEM('',(#13074),#318);
#307=STYLED_ITEM('',(#13074),#319);
#308=STYLED_ITEM('',(#13075),#320);
#309=STYLED_ITEM('',(#13076),#321);
#310=STYLED_ITEM('',(#13077),#322);
#311=STYLED_ITEM('',(#13075),#323);
#312=STYLED_ITEM('',(#13075),#324);
#313=STYLED_ITEM('',(#13075),#325);
#314=STYLED_ITEM('',(#13075),#326);
#315=MANIFOLD_SOLID_BREP('Body1',#5578);
#316=MANIFOLD_SOLID_BREP('Body2',#5579);
#317=MANIFOLD_SOLID_BREP('Body3',#5580);
#318=MANIFOLD_SOLID_BREP('Body4',#5581);
#319=MANIFOLD_SOLID_BREP('Body5',#5582);
#320=MANIFOLD_SOLID_BREP('Body1',#5583);
#321=MANIFOLD_SOLID_BREP('Body1',#5584);
#322=MANIFOLD_SOLID_BREP('Body1',#5585);
#323=MANIFOLD_SOLID_BREP('Body1',#5586);
#324=MANIFOLD_SOLID_BREP('Body1',#5587);
#325=MANIFOLD_SOLID_BREP('Body1',#5588);
#326=MANIFOLD_SOLID_BREP('Body1',#5589);
#327=FACE_BOUND('',#877,.T.);
#328=FACE_BOUND('',#878,.T.);
#329=FACE_BOUND('',#879,.T.);
#330=FACE_BOUND('',#880,.T.);
#331=FACE_BOUND('',#881,.T.);
#332=FACE_BOUND('',#882,.T.);
#333=FACE_BOUND('',#883,.T.);
#334=FACE_BOUND('',#885,.T.);
#335=FACE_BOUND('',#886,.T.);
#336=FACE_BOUND('',#887,.T.);
#337=FACE_BOUND('',#888,.T.);
#338=FACE_BOUND('',#889,.T.);
#339=FACE_BOUND('',#890,.T.);
#340=FACE_BOUND('',#891,.T.);
#341=FACE_BOUND('',#908,.T.);
#342=FACE_BOUND('',#909,.T.);
#343=FACE_BOUND('',#910,.T.);
#344=FACE_BOUND('',#911,.T.);
#345=FACE_BOUND('',#912,.T.);
#346=FACE_BOUND('',#913,.T.);
#347=FACE_BOUND('',#914,.T.);
#348=FACE_BOUND('',#916,.T.);
#349=FACE_BOUND('',#917,.T.);
#350=FACE_BOUND('',#918,.T.);
#351=FACE_BOUND('',#919,.T.);
#352=FACE_BOUND('',#920,.T.);
#353=FACE_BOUND('',#921,.T.);
#354=FACE_BOUND('',#922,.T.);
#355=FACE_BOUND('',#953,.T.);
#356=FACE_BOUND('',#955,.T.);
#357=FACE_BOUND('',#957,.T.);
#358=FACE_BOUND('',#958,.T.);
#359=FACE_BOUND('',#959,.T.);
#360=FACE_BOUND('',#960,.T.);
#361=FACE_BOUND('',#962,.T.);
#362=FACE_BOUND('',#963,.T.);
#363=FACE_BOUND('',#964,.T.);
#364=FACE_BOUND('',#965,.T.);
#365=FACE_BOUND('',#1007,.T.);
#366=FACE_BOUND('',#1016,.T.);
#367=FACE_BOUND('',#1036,.T.);
#368=FACE_BOUND('',#1038,.T.);
#369=FACE_BOUND('',#1040,.T.);
#370=FACE_BOUND('',#1042,.T.);
#371=FACE_BOUND('',#1123,.T.);
#372=FACE_BOUND('',#1125,.T.);
#373=FACE_BOUND('',#1129,.T.);
#374=FACE_BOUND('',#1130,.T.);
#375=FACE_BOUND('',#1132,.T.);
#376=FACE_BOUND('',#1133,.T.);
#377=FACE_BOUND('',#1144,.T.);
#378=FACE_BOUND('',#1146,.T.);
#379=FACE_BOUND('',#1148,.T.);
#380=FACE_BOUND('',#1168,.T.);
#381=FACE_BOUND('',#1170,.T.);
#382=FACE_BOUND('',#1172,.T.);
#383=FACE_BOUND('',#1192,.T.);
#384=FACE_BOUND('',#1194,.T.);
#385=FACE_BOUND('',#1196,.T.);
#386=FACE_BOUND('',#1216,.T.);
#387=FACE_BOUND('',#1218,.T.);
#388=FACE_BOUND('',#1220,.T.);
#389=PLANE('',#5705);
#390=PLANE('',#5709);
#391=PLANE('',#5713);
#392=PLANE('',#5717);
#393=PLANE('',#5718);
#394=PLANE('',#5719);
#395=PLANE('',#5744);
#396=PLANE('',#5748);
#397=PLANE('',#5752);
#398=PLANE('',#5756);
#399=PLANE('',#5757);
#400=PLANE('',#5758);
#401=PLANE('',#5759);
#402=PLANE('',#5760);
#403=PLANE('',#5761);
#404=PLANE('',#5762);
#405=PLANE('',#5763);
#406=PLANE('',#5764);
#407=PLANE('',#5765);
#408=PLANE('',#5766);
#409=PLANE('',#5767);
#410=PLANE('',#5768);
#411=PLANE('',#5769);
#412=PLANE('',#5770);
#413=PLANE('',#5771);
#414=PLANE('',#5772);
#415=PLANE('',#5773);
#416=PLANE('',#5774);
#417=PLANE('',#5775);
#418=PLANE('',#5776);
#419=PLANE('',#5777);
#420=PLANE('',#5778);
#421=PLANE('',#5779);
#422=PLANE('',#5780);
#423=PLANE('',#5781);
#424=PLANE('',#5782);
#425=PLANE('',#5799);
#426=PLANE('',#5800);
#427=PLANE('',#5801);
#428=PLANE('',#5809);
#429=PLANE('',#5816);
#430=PLANE('',#5817);
#431=PLANE('',#5819);
#432=PLANE('',#5821);
#433=PLANE('',#5822);
#434=PLANE('',#5823);
#435=PLANE('',#5824);
#436=PLANE('',#5825);
#437=PLANE('',#5826);
#438=PLANE('',#5828);
#439=PLANE('',#5829);
#440=PLANE('',#5830);
#441=PLANE('',#5831);
#442=PLANE('',#5832);
#443=PLANE('',#5833);
#444=PLANE('',#5834);
#445=PLANE('',#5835);
#446=PLANE('',#5836);
#447=PLANE('',#5837);
#448=PLANE('',#5838);
#449=PLANE('',#5839);
#450=PLANE('',#5842);
#451=PLANE('',#5843);
#452=PLANE('',#5844);
#453=PLANE('',#5845);
#454=PLANE('',#5848);
#455=PLANE('',#5849);
#456=PLANE('',#5852);
#457=PLANE('',#5853);
#458=PLANE('',#5854);
#459=PLANE('',#5855);
#460=PLANE('',#5858);
#461=PLANE('',#5859);
#462=PLANE('',#5860);
#463=PLANE('',#5861);
#464=PLANE('',#5862);
#465=PLANE('',#5865);
#466=PLANE('',#5866);
#467=PLANE('',#5867);
#468=PLANE('',#5868);
#469=PLANE('',#5869);
#470=PLANE('',#5870);
#471=PLANE('',#5871);
#472=PLANE('',#5874);
#473=PLANE('',#5875);
#474=PLANE('',#5876);
#475=PLANE('',#5877);
#476=PLANE('',#5878);
#477=PLANE('',#5879);
#478=PLANE('',#5882);
#479=PLANE('',#5883);
#480=PLANE('',#5903);
#481=PLANE('',#5904);
#482=PLANE('',#5905);
#483=PLANE('',#5945);
#484=PLANE('',#6024);
#485=PLANE('',#6025);
#486=PLANE('',#6033);
#487=PLANE('',#6036);
#488=PLANE('',#6040);
#489=PLANE('',#6042);
#490=PLANE('',#6064);
#491=PLANE('',#6065);
#492=PLANE('',#6066);
#493=PLANE('',#6067);
#494=PLANE('',#6068);
#495=PLANE('',#6069);
#496=PLANE('',#6070);
#497=PLANE('',#6071);
#498=PLANE('',#6072);
#499=PLANE('',#6073);
#500=PLANE('',#6074);
#501=PLANE('',#6075);
#502=PLANE('',#6076);
#503=PLANE('',#6077);
#504=PLANE('',#6078);
#505=PLANE('',#6100);
#506=PLANE('',#6101);
#507=PLANE('',#6102);
#508=PLANE('',#6103);
#509=PLANE('',#6104);
#510=PLANE('',#6105);
#511=PLANE('',#6106);
#512=PLANE('',#6107);
#513=PLANE('',#6108);
#514=PLANE('',#6109);
#515=PLANE('',#6110);
#516=PLANE('',#6111);
#517=PLANE('',#6112);
#518=PLANE('',#6113);
#519=PLANE('',#6114);
#520=PLANE('',#6136);
#521=PLANE('',#6137);
#522=PLANE('',#6138);
#523=PLANE('',#6139);
#524=PLANE('',#6140);
#525=PLANE('',#6141);
#526=PLANE('',#6142);
#527=PLANE('',#6143);
#528=PLANE('',#6144);
#529=PLANE('',#6145);
#530=PLANE('',#6146);
#531=PLANE('',#6147);
#532=PLANE('',#6148);
#533=PLANE('',#6149);
#534=PLANE('',#6150);
#535=PLANE('',#6172);
#536=PLANE('',#6173);
#537=PLANE('',#6174);
#538=PLANE('',#6175);
#539=PLANE('',#6176);
#540=PLANE('',#6177);
#541=PLANE('',#6178);
#542=PLANE('',#6179);
#543=PLANE('',#6180);
#544=PLANE('',#6181);
#545=PLANE('',#6182);
#546=PLANE('',#6183);
#547=PLANE('',#6184);
#548=PLANE('',#6185);
#549=PLANE('',#6186);
#550=FACE_OUTER_BOUND('',#861,.T.);
#551=FACE_OUTER_BOUND('',#862,.T.);
#552=FACE_OUTER_BOUND('',#863,.T.);
#553=FACE_OUTER_BOUND('',#864,.T.);
#554=FACE_OUTER_BOUND('',#865,.T.);
#555=FACE_OUTER_BOUND('',#866,.T.);
#556=FACE_OUTER_BOUND('',#867,.T.);
#557=FACE_OUTER_BOUND('',#868,.T.);
#558=FACE_OUTER_BOUND('',#869,.T.);
#559=FACE_OUTER_BOUND('',#870,.T.);
#560=FACE_OUTER_BOUND('',#871,.T.);
#561=FACE_OUTER_BOUND('',#872,.T.);
#562=FACE_OUTER_BOUND('',#873,.T.);
#563=FACE_OUTER_BOUND('',#874,.T.);
#564=FACE_OUTER_BOUND('',#875,.T.);
#565=FACE_OUTER_BOUND('',#876,.T.);
#566=FACE_OUTER_BOUND('',#884,.T.);
#567=FACE_OUTER_BOUND('',#892,.T.);
#568=FACE_OUTER_BOUND('',#893,.T.);
#569=FACE_OUTER_BOUND('',#894,.T.);
#570=FACE_OUTER_BOUND('',#895,.T.);
#571=FACE_OUTER_BOUND('',#896,.T.);
#572=FACE_OUTER_BOUND('',#897,.T.);
#573=FACE_OUTER_BOUND('',#898,.T.);
#574=FACE_OUTER_BOUND('',#899,.T.);
#575=FACE_OUTER_BOUND('',#900,.T.);
#576=FACE_OUTER_BOUND('',#901,.T.);
#577=FACE_OUTER_BOUND('',#902,.T.);
#578=FACE_OUTER_BOUND('',#903,.T.);
#579=FACE_OUTER_BOUND('',#904,.T.);
#580=FACE_OUTER_BOUND('',#905,.T.);
#581=FACE_OUTER_BOUND('',#906,.T.);
#582=FACE_OUTER_BOUND('',#907,.T.);
#583=FACE_OUTER_BOUND('',#915,.T.);
#584=FACE_OUTER_BOUND('',#923,.T.);
#585=FACE_OUTER_BOUND('',#924,.T.);
#586=FACE_OUTER_BOUND('',#925,.T.);
#587=FACE_OUTER_BOUND('',#926,.T.);
#588=FACE_OUTER_BOUND('',#927,.T.);
#589=FACE_OUTER_BOUND('',#928,.T.);
#590=FACE_OUTER_BOUND('',#929,.T.);
#591=FACE_OUTER_BOUND('',#930,.T.);
#592=FACE_OUTER_BOUND('',#931,.T.);
#593=FACE_OUTER_BOUND('',#932,.T.);
#594=FACE_OUTER_BOUND('',#933,.T.);
#595=FACE_OUTER_BOUND('',#934,.T.);
#596=FACE_OUTER_BOUND('',#935,.T.);
#597=FACE_OUTER_BOUND('',#936,.T.);
#598=FACE_OUTER_BOUND('',#937,.T.);
#599=FACE_OUTER_BOUND('',#938,.T.);
#600=FACE_OUTER_BOUND('',#939,.T.);
#601=FACE_OUTER_BOUND('',#940,.T.);
#602=FACE_OUTER_BOUND('',#941,.T.);
#603=FACE_OUTER_BOUND('',#942,.T.);
#604=FACE_OUTER_BOUND('',#943,.T.);
#605=FACE_OUTER_BOUND('',#944,.T.);
#606=FACE_OUTER_BOUND('',#945,.T.);
#607=FACE_OUTER_BOUND('',#946,.T.);
#608=FACE_OUTER_BOUND('',#947,.T.);
#609=FACE_OUTER_BOUND('',#948,.T.);
#610=FACE_OUTER_BOUND('',#949,.T.);
#611=FACE_OUTER_BOUND('',#950,.T.);
#612=FACE_OUTER_BOUND('',#951,.T.);
#613=FACE_OUTER_BOUND('',#952,.T.);
#614=FACE_OUTER_BOUND('',#954,.T.);
#615=FACE_OUTER_BOUND('',#956,.T.);
#616=FACE_OUTER_BOUND('',#961,.T.);
#617=FACE_OUTER_BOUND('',#966,.T.);
#618=FACE_OUTER_BOUND('',#967,.T.);
#619=FACE_OUTER_BOUND('',#968,.T.);
#620=FACE_OUTER_BOUND('',#969,.T.);
#621=FACE_OUTER_BOUND('',#970,.T.);
#622=FACE_OUTER_BOUND('',#971,.T.);
#623=FACE_OUTER_BOUND('',#972,.T.);
#624=FACE_OUTER_BOUND('',#973,.T.);
#625=FACE_OUTER_BOUND('',#974,.T.);
#626=FACE_OUTER_BOUND('',#975,.T.);
#627=FACE_OUTER_BOUND('',#976,.T.);
#628=FACE_OUTER_BOUND('',#977,.T.);
#629=FACE_OUTER_BOUND('',#978,.T.);
#630=FACE_OUTER_BOUND('',#979,.T.);
#631=FACE_OUTER_BOUND('',#980,.T.);
#632=FACE_OUTER_BOUND('',#981,.T.);
#633=FACE_OUTER_BOUND('',#982,.T.);
#634=FACE_OUTER_BOUND('',#983,.T.);
#635=FACE_OUTER_BOUND('',#984,.T.);
#636=FACE_OUTER_BOUND('',#985,.T.);
#637=FACE_OUTER_BOUND('',#986,.T.);
#638=FACE_OUTER_BOUND('',#987,.T.);
#639=FACE_OUTER_BOUND('',#988,.T.);
#640=FACE_OUTER_BOUND('',#989,.T.);
#641=FACE_OUTER_BOUND('',#990,.T.);
#642=FACE_OUTER_BOUND('',#991,.T.);
#643=FACE_OUTER_BOUND('',#992,.T.);
#644=FACE_OUTER_BOUND('',#993,.T.);
#645=FACE_OUTER_BOUND('',#994,.T.);
#646=FACE_OUTER_BOUND('',#995,.T.);
#647=FACE_OUTER_BOUND('',#996,.T.);
#648=FACE_OUTER_BOUND('',#997,.T.);
#649=FACE_OUTER_BOUND('',#998,.T.);
#650=FACE_OUTER_BOUND('',#999,.T.);
#651=FACE_OUTER_BOUND('',#1000,.T.);
#652=FACE_OUTER_BOUND('',#1001,.T.);
#653=FACE_OUTER_BOUND('',#1002,.T.);
#654=FACE_OUTER_BOUND('',#1003,.T.);
#655=FACE_OUTER_BOUND('',#1004,.T.);
#656=FACE_OUTER_BOUND('',#1005,.T.);
#657=FACE_OUTER_BOUND('',#1006,.T.);
#658=FACE_OUTER_BOUND('',#1008,.T.);
#659=FACE_OUTER_BOUND('',#1009,.T.);
#660=FACE_OUTER_BOUND('',#1010,.T.);
#661=FACE_OUTER_BOUND('',#1011,.T.);
#662=FACE_OUTER_BOUND('',#1012,.T.);
#663=FACE_OUTER_BOUND('',#1013,.T.);
#664=FACE_OUTER_BOUND('',#1014,.T.);
#665=FACE_OUTER_BOUND('',#1015,.T.);
#666=FACE_OUTER_BOUND('',#1017,.T.);
#667=FACE_OUTER_BOUND('',#1018,.T.);
#668=FACE_OUTER_BOUND('',#1019,.T.);
#669=FACE_OUTER_BOUND('',#1020,.T.);
#670=FACE_OUTER_BOUND('',#1021,.T.);
#671=FACE_OUTER_BOUND('',#1022,.T.);
#672=FACE_OUTER_BOUND('',#1023,.T.);
#673=FACE_OUTER_BOUND('',#1024,.T.);
#674=FACE_OUTER_BOUND('',#1025,.T.);
#675=FACE_OUTER_BOUND('',#1026,.T.);
#676=FACE_OUTER_BOUND('',#1027,.T.);
#677=FACE_OUTER_BOUND('',#1028,.T.);
#678=FACE_OUTER_BOUND('',#1029,.T.);
#679=FACE_OUTER_BOUND('',#1030,.T.);
#680=FACE_OUTER_BOUND('',#1031,.T.);
#681=FACE_OUTER_BOUND('',#1032,.T.);
#682=FACE_OUTER_BOUND('',#1033,.T.);
#683=FACE_OUTER_BOUND('',#1034,.T.);
#684=FACE_OUTER_BOUND('',#1035,.T.);
#685=FACE_OUTER_BOUND('',#1037,.T.);
#686=FACE_OUTER_BOUND('',#1039,.T.);
#687=FACE_OUTER_BOUND('',#1041,.T.);
#688=FACE_OUTER_BOUND('',#1043,.T.);
#689=FACE_OUTER_BOUND('',#1044,.T.);
#690=FACE_OUTER_BOUND('',#1045,.T.);
#691=FACE_OUTER_BOUND('',#1046,.T.);
#692=FACE_OUTER_BOUND('',#1047,.T.);
#693=FACE_OUTER_BOUND('',#1048,.T.);
#694=FACE_OUTER_BOUND('',#1049,.T.);
#695=FACE_OUTER_BOUND('',#1050,.T.);
#696=FACE_OUTER_BOUND('',#1051,.T.);
#697=FACE_OUTER_BOUND('',#1052,.T.);
#698=FACE_OUTER_BOUND('',#1053,.T.);
#699=FACE_OUTER_BOUND('',#1054,.T.);
#700=FACE_OUTER_BOUND('',#1055,.T.);
#701=FACE_OUTER_BOUND('',#1056,.T.);
#702=FACE_OUTER_BOUND('',#1057,.T.);
#703=FACE_OUTER_BOUND('',#1058,.T.);
#704=FACE_OUTER_BOUND('',#1059,.T.);
#705=FACE_OUTER_BOUND('',#1060,.T.);
#706=FACE_OUTER_BOUND('',#1061,.T.);
#707=FACE_OUTER_BOUND('',#1062,.T.);
#708=FACE_OUTER_BOUND('',#1063,.T.);
#709=FACE_OUTER_BOUND('',#1064,.T.);
#710=FACE_OUTER_BOUND('',#1065,.T.);
#711=FACE_OUTER_BOUND('',#1066,.T.);
#712=FACE_OUTER_BOUND('',#1067,.T.);
#713=FACE_OUTER_BOUND('',#1068,.T.);
#714=FACE_OUTER_BOUND('',#1069,.T.);
#715=FACE_OUTER_BOUND('',#1070,.T.);
#716=FACE_OUTER_BOUND('',#1071,.T.);
#717=FACE_OUTER_BOUND('',#1072,.T.);
#718=FACE_OUTER_BOUND('',#1073,.T.);
#719=FACE_OUTER_BOUND('',#1074,.T.);
#720=FACE_OUTER_BOUND('',#1075,.T.);
#721=FACE_OUTER_BOUND('',#1076,.T.);
#722=FACE_OUTER_BOUND('',#1077,.T.);
#723=FACE_OUTER_BOUND('',#1078,.T.);
#724=FACE_OUTER_BOUND('',#1079,.T.);
#725=FACE_OUTER_BOUND('',#1080,.T.);
#726=FACE_OUTER_BOUND('',#1081,.T.);
#727=FACE_OUTER_BOUND('',#1082,.T.);
#728=FACE_OUTER_BOUND('',#1083,.T.);
#729=FACE_OUTER_BOUND('',#1084,.T.);
#730=FACE_OUTER_BOUND('',#1085,.T.);
#731=FACE_OUTER_BOUND('',#1086,.T.);
#732=FACE_OUTER_BOUND('',#1087,.T.);
#733=FACE_OUTER_BOUND('',#1088,.T.);
#734=FACE_OUTER_BOUND('',#1089,.T.);
#735=FACE_OUTER_BOUND('',#1090,.T.);
#736=FACE_OUTER_BOUND('',#1091,.T.);
#737=FACE_OUTER_BOUND('',#1092,.T.);
#738=FACE_OUTER_BOUND('',#1093,.T.);
#739=FACE_OUTER_BOUND('',#1094,.T.);
#740=FACE_OUTER_BOUND('',#1095,.T.);
#741=FACE_OUTER_BOUND('',#1096,.T.);
#742=FACE_OUTER_BOUND('',#1097,.T.);
#743=FACE_OUTER_BOUND('',#1098,.T.);
#744=FACE_OUTER_BOUND('',#1099,.T.);
#745=FACE_OUTER_BOUND('',#1100,.T.);
#746=FACE_OUTER_BOUND('',#1101,.T.);
#747=FACE_OUTER_BOUND('',#1102,.T.);
#748=FACE_OUTER_BOUND('',#1103,.T.);
#749=FACE_OUTER_BOUND('',#1104,.T.);
#750=FACE_OUTER_BOUND('',#1105,.T.);
#751=FACE_OUTER_BOUND('',#1106,.T.);
#752=FACE_OUTER_BOUND('',#1107,.T.);
#753=FACE_OUTER_BOUND('',#1108,.T.);
#754=FACE_OUTER_BOUND('',#1109,.T.);
#755=FACE_OUTER_BOUND('',#1110,.T.);
#756=FACE_OUTER_BOUND('',#1111,.T.);
#757=FACE_OUTER_BOUND('',#1112,.T.);
#758=FACE_OUTER_BOUND('',#1113,.T.);
#759=FACE_OUTER_BOUND('',#1114,.T.);
#760=FACE_OUTER_BOUND('',#1115,.T.);
#761=FACE_OUTER_BOUND('',#1116,.T.);
#762=FACE_OUTER_BOUND('',#1117,.T.);
#763=FACE_OUTER_BOUND('',#1118,.T.);
#764=FACE_OUTER_BOUND('',#1119,.T.);
#765=FACE_OUTER_BOUND('',#1120,.T.);
#766=FACE_OUTER_BOUND('',#1121,.T.);
#767=FACE_OUTER_BOUND('',#1122,.T.);
#768=FACE_OUTER_BOUND('',#1124,.T.);
#769=FACE_OUTER_BOUND('',#1126,.T.);
#770=FACE_OUTER_BOUND('',#1127,.T.);
#771=FACE_OUTER_BOUND('',#1128,.T.);
#772=FACE_OUTER_BOUND('',#1131,.T.);
#773=FACE_OUTER_BOUND('',#1134,.T.);
#774=FACE_OUTER_BOUND('',#1135,.T.);
#775=FACE_OUTER_BOUND('',#1136,.T.);
#776=FACE_OUTER_BOUND('',#1137,.T.);
#777=FACE_OUTER_BOUND('',#1138,.T.);
#778=FACE_OUTER_BOUND('',#1139,.T.);
#779=FACE_OUTER_BOUND('',#1140,.T.);
#780=FACE_OUTER_BOUND('',#1141,.T.);
#781=FACE_OUTER_BOUND('',#1142,.T.);
#782=FACE_OUTER_BOUND('',#1143,.T.);
#783=FACE_OUTER_BOUND('',#1145,.T.);
#784=FACE_OUTER_BOUND('',#1147,.T.);
#785=FACE_OUTER_BOUND('',#1149,.T.);
#786=FACE_OUTER_BOUND('',#1150,.T.);
#787=FACE_OUTER_BOUND('',#1151,.T.);
#788=FACE_OUTER_BOUND('',#1152,.T.);
#789=FACE_OUTER_BOUND('',#1153,.T.);
#790=FACE_OUTER_BOUND('',#1154,.T.);
#791=FACE_OUTER_BOUND('',#1155,.T.);
#792=FACE_OUTER_BOUND('',#1156,.T.);
#793=FACE_OUTER_BOUND('',#1157,.T.);
#794=FACE_OUTER_BOUND('',#1158,.T.);
#795=FACE_OUTER_BOUND('',#1159,.T.);
#796=FACE_OUTER_BOUND('',#1160,.T.);
#797=FACE_OUTER_BOUND('',#1161,.T.);
#798=FACE_OUTER_BOUND('',#1162,.T.);
#799=FACE_OUTER_BOUND('',#1163,.T.);
#800=FACE_OUTER_BOUND('',#1164,.T.);
#801=FACE_OUTER_BOUND('',#1165,.T.);
#802=FACE_OUTER_BOUND('',#1166,.T.);
#803=FACE_OUTER_BOUND('',#1167,.T.);
#804=FACE_OUTER_BOUND('',#1169,.T.);
#805=FACE_OUTER_BOUND('',#1171,.T.);
#806=FACE_OUTER_BOUND('',#1173,.T.);
#807=FACE_OUTER_BOUND('',#1174,.T.);
#808=FACE_OUTER_BOUND('',#1175,.T.);
#809=FACE_OUTER_BOUND('',#1176,.T.);
#810=FACE_OUTER_BOUND('',#1177,.T.);
#811=FACE_OUTER_BOUND('',#1178,.T.);
#812=FACE_OUTER_BOUND('',#1179,.T.);
#813=FACE_OUTER_BOUND('',#1180,.T.);
#814=FACE_OUTER_BOUND('',#1181,.T.);
#815=FACE_OUTER_BOUND('',#1182,.T.);
#816=FACE_OUTER_BOUND('',#1183,.T.);
#817=FACE_OUTER_BOUND('',#1184,.T.);
#818=FACE_OUTER_BOUND('',#1185,.T.);
#819=FACE_OUTER_BOUND('',#1186,.T.);
#820=FACE_OUTER_BOUND('',#1187,.T.);
#821=FACE_OUTER_BOUND('',#1188,.T.);
#822=FACE_OUTER_BOUND('',#1189,.T.);
#823=FACE_OUTER_BOUND('',#1190,.T.);
#824=FACE_OUTER_BOUND('',#1191,.T.);
#825=FACE_OUTER_BOUND('',#1193,.T.);
#826=FACE_OUTER_BOUND('',#1195,.T.);
#827=FACE_OUTER_BOUND('',#1197,.T.);
#828=FACE_OUTER_BOUND('',#1198,.T.);
#829=FACE_OUTER_BOUND('',#1199,.T.);
#830=FACE_OUTER_BOUND('',#1200,.T.);
#831=FACE_OUTER_BOUND('',#1201,.T.);
#832=FACE_OUTER_BOUND('',#1202,.T.);
#833=FACE_OUTER_BOUND('',#1203,.T.);
#834=FACE_OUTER_BOUND('',#1204,.T.);
#835=FACE_OUTER_BOUND('',#1205,.T.);
#836=FACE_OUTER_BOUND('',#1206,.T.);
#837=FACE_OUTER_BOUND('',#1207,.T.);
#838=FACE_OUTER_BOUND('',#1208,.T.);
#839=FACE_OUTER_BOUND('',#1209,.T.);
#840=FACE_OUTER_BOUND('',#1210,.T.);
#841=FACE_OUTER_BOUND('',#1211,.T.);
#842=FACE_OUTER_BOUND('',#1212,.T.);
#843=FACE_OUTER_BOUND('',#1213,.T.);
#844=FACE_OUTER_BOUND('',#1214,.T.);
#845=FACE_OUTER_BOUND('',#1215,.T.);
#846=FACE_OUTER_BOUND('',#1217,.T.);
#847=FACE_OUTER_BOUND('',#1219,.T.);
#848=FACE_OUTER_BOUND('',#1221,.T.);
#849=FACE_OUTER_BOUND('',#1222,.T.);
#850=FACE_OUTER_BOUND('',#1223,.T.);
#851=FACE_OUTER_BOUND('',#1224,.T.);
#852=FACE_OUTER_BOUND('',#1225,.T.);
#853=FACE_OUTER_BOUND('',#1226,.T.);
#854=FACE_OUTER_BOUND('',#1227,.T.);
#855=FACE_OUTER_BOUND('',#1228,.T.);
#856=FACE_OUTER_BOUND('',#1229,.T.);
#857=FACE_OUTER_BOUND('',#1230,.T.);
#858=FACE_OUTER_BOUND('',#1231,.T.);
#859=FACE_OUTER_BOUND('',#1232,.T.);
#860=FACE_OUTER_BOUND('',#1233,.T.);
#861=EDGE_LOOP('',(#3643,#3644,#3645,#3646));
#862=EDGE_LOOP('',(#3647,#3648,#3649,#3650));
#863=EDGE_LOOP('',(#3651,#3652,#3653,#3654));
#864=EDGE_LOOP('',(#3655,#3656,#3657,#3658));
#865=EDGE_LOOP('',(#3659,#3660,#3661,#3662));
#866=EDGE_LOOP('',(#3663,#3664,#3665,#3666));
#867=EDGE_LOOP('',(#3667,#3668,#3669,#3670));
#868=EDGE_LOOP('',(#3671,#3672,#3673,#3674));
#869=EDGE_LOOP('',(#3675,#3676,#3677,#3678));
#870=EDGE_LOOP('',(#3679,#3680,#3681,#3682));
#871=EDGE_LOOP('',(#3683,#3684,#3685,#3686));
#872=EDGE_LOOP('',(#3687,#3688,#3689,#3690));
#873=EDGE_LOOP('',(#3691,#3692,#3693,#3694));
#874=EDGE_LOOP('',(#3695,#3696,#3697,#3698));
#875=EDGE_LOOP('',(#3699,#3700,#3701,#3702));
#876=EDGE_LOOP('',(#3703,#3704,#3705,#3706,#3707,#3708,#3709,#3710));
#877=EDGE_LOOP('',(#3711));
#878=EDGE_LOOP('',(#3712));
#879=EDGE_LOOP('',(#3713));
#880=EDGE_LOOP('',(#3714));
#881=EDGE_LOOP('',(#3715));
#882=EDGE_LOOP('',(#3716));
#883=EDGE_LOOP('',(#3717));
#884=EDGE_LOOP('',(#3718,#3719,#3720,#3721,#3722,#3723,#3724,#3725));
#885=EDGE_LOOP('',(#3726));
#886=EDGE_LOOP('',(#3727));
#887=EDGE_LOOP('',(#3728));
#888=EDGE_LOOP('',(#3729));
#889=EDGE_LOOP('',(#3730));
#890=EDGE_LOOP('',(#3731));
#891=EDGE_LOOP('',(#3732));
#892=EDGE_LOOP('',(#3733,#3734,#3735,#3736));
#893=EDGE_LOOP('',(#3737,#3738,#3739,#3740));
#894=EDGE_LOOP('',(#3741,#3742,#3743,#3744));
#895=EDGE_LOOP('',(#3745,#3746,#3747,#3748));
#896=EDGE_LOOP('',(#3749,#3750,#3751,#3752));
#897=EDGE_LOOP('',(#3753,#3754,#3755,#3756));
#898=EDGE_LOOP('',(#3757,#3758,#3759,#3760));
#899=EDGE_LOOP('',(#3761,#3762,#3763,#3764));
#900=EDGE_LOOP('',(#3765,#3766,#3767,#3768));
#901=EDGE_LOOP('',(#3769,#3770,#3771,#3772));
#902=EDGE_LOOP('',(#3773,#3774,#3775,#3776));
#903=EDGE_LOOP('',(#3777,#3778,#3779,#3780));
#904=EDGE_LOOP('',(#3781,#3782,#3783,#3784));
#905=EDGE_LOOP('',(#3785,#3786,#3787,#3788));
#906=EDGE_LOOP('',(#3789,#3790,#3791,#3792));
#907=EDGE_LOOP('',(#3793,#3794,#3795,#3796,#3797,#3798,#3799,#3800));
#908=EDGE_LOOP('',(#3801));
#909=EDGE_LOOP('',(#3802));
#910=EDGE_LOOP('',(#3803));
#911=EDGE_LOOP('',(#3804));
#912=EDGE_LOOP('',(#3805));
#913=EDGE_LOOP('',(#3806));
#914=EDGE_LOOP('',(#3807));
#915=EDGE_LOOP('',(#3808,#3809,#3810,#3811,#3812,#3813,#3814,#3815));
#916=EDGE_LOOP('',(#3816));
#917=EDGE_LOOP('',(#3817));
#918=EDGE_LOOP('',(#3818));
#919=EDGE_LOOP('',(#3819));
#920=EDGE_LOOP('',(#3820));
#921=EDGE_LOOP('',(#3821));
#922=EDGE_LOOP('',(#3822));
#923=EDGE_LOOP('',(#3823,#3824,#3825,#3826));
#924=EDGE_LOOP('',(#3827,#3828,#3829,#3830));
#925=EDGE_LOOP('',(#3831,#3832,#3833,#3834));
#926=EDGE_LOOP('',(#3835,#3836,#3837,#3838));
#927=EDGE_LOOP('',(#3839,#3840,#3841,#3842));
#928=EDGE_LOOP('',(#3843,#3844,#3845,#3846));
#929=EDGE_LOOP('',(#3847,#3848,#3849,#3850,#3851,#3852));
#930=EDGE_LOOP('',(#3853,#3854,#3855,#3856,#3857,#3858));
#931=EDGE_LOOP('',(#3859,#3860,#3861,#3862));
#932=EDGE_LOOP('',(#3863,#3864,#3865,#3866));
#933=EDGE_LOOP('',(#3867,#3868,#3869,#3870));
#934=EDGE_LOOP('',(#3871,#3872,#3873,#3874));
#935=EDGE_LOOP('',(#3875,#3876,#3877,#3878));
#936=EDGE_LOOP('',(#3879,#3880,#3881,#3882));
#937=EDGE_LOOP('',(#3883,#3884,#3885,#3886,#3887,#3888));
#938=EDGE_LOOP('',(#3889,#3890,#3891,#3892,#3893,#3894));
#939=EDGE_LOOP('',(#3895,#3896,#3897,#3898));
#940=EDGE_LOOP('',(#3899,#3900,#3901,#3902));
#941=EDGE_LOOP('',(#3903,#3904,#3905,#3906));
#942=EDGE_LOOP('',(#3907,#3908,#3909,#3910));
#943=EDGE_LOOP('',(#3911,#3912,#3913,#3914));
#944=EDGE_LOOP('',(#3915,#3916,#3917,#3918));
#945=EDGE_LOOP('',(#3919,#3920,#3921,#3922,#3923,#3924));
#946=EDGE_LOOP('',(#3925,#3926,#3927,#3928,#3929,#3930));
#947=EDGE_LOOP('',(#3931,#3932,#3933,#3934));
#948=EDGE_LOOP('',(#3935,#3936,#3937,#3938));
#949=EDGE_LOOP('',(#3939,#3940,#3941,#3942));
#950=EDGE_LOOP('',(#3943,#3944,#3945,#3946));
#951=EDGE_LOOP('',(#3947,#3948,#3949,#3950));
#952=EDGE_LOOP('',(#3951));
#953=EDGE_LOOP('',(#3952));
#954=EDGE_LOOP('',(#3953));
#955=EDGE_LOOP('',(#3954));
#956=EDGE_LOOP('',(#3955,#3956,#3957,#3958,#3959,#3960,#3961,#3962,#3963,
#3964,#3965,#3966,#3967,#3968,#3969,#3970,#3971,#3972,#3973,#3974));
#957=EDGE_LOOP('',(#3975,#3976,#3977,#3978,#3979,#3980,#3981,#3982));
#958=EDGE_LOOP('',(#3983,#3984,#3985,#3986,#3987));
#959=EDGE_LOOP('',(#3988,#3989,#3990,#3991,#3992));
#960=EDGE_LOOP('',(#3993));
#961=EDGE_LOOP('',(#3994,#3995,#3996,#3997,#3998,#3999,#4000,#4001,#4002,
#4003,#4004,#4005,#4006,#4007,#4008,#4009,#4010,#4011,#4012,#4013));
#962=EDGE_LOOP('',(#4014,#4015,#4016,#4017,#4018));
#963=EDGE_LOOP('',(#4019,#4020,#4021,#4022,#4023));
#964=EDGE_LOOP('',(#4024,#4025,#4026,#4027,#4028,#4029,#4030,#4031));
#965=EDGE_LOOP('',(#4032));
#966=EDGE_LOOP('',(#4033,#4034,#4035,#4036));
#967=EDGE_LOOP('',(#4037,#4038,#4039,#4040));
#968=EDGE_LOOP('',(#4041,#4042,#4043,#4044));
#969=EDGE_LOOP('',(#4045,#4046,#4047,#4048));
#970=EDGE_LOOP('',(#4049,#4050,#4051,#4052));
#971=EDGE_LOOP('',(#4053,#4054,#4055,#4056));
#972=EDGE_LOOP('',(#4057,#4058,#4059,#4060));
#973=EDGE_LOOP('',(#4061,#4062,#4063,#4064));
#974=EDGE_LOOP('',(#4065,#4066,#4067,#4068));
#975=EDGE_LOOP('',(#4069,#4070,#4071,#4072));
#976=EDGE_LOOP('',(#4073,#4074,#4075,#4076));
#977=EDGE_LOOP('',(#4077,#4078,#4079,#4080));
#978=EDGE_LOOP('',(#4081,#4082,#4083,#4084));
#979=EDGE_LOOP('',(#4085,#4086,#4087,#4088));
#980=EDGE_LOOP('',(#4089,#4090,#4091,#4092));
#981=EDGE_LOOP('',(#4093,#4094,#4095,#4096));
#982=EDGE_LOOP('',(#4097,#4098,#4099,#4100));
#983=EDGE_LOOP('',(#4101,#4102,#4103,#4104));
#984=EDGE_LOOP('',(#4105,#4106,#4107,#4108));
#985=EDGE_LOOP('',(#4109,#4110,#4111,#4112));
#986=EDGE_LOOP('',(#4113,#4114,#4115,#4116));
#987=EDGE_LOOP('',(#4117,#4118,#4119,#4120));
#988=EDGE_LOOP('',(#4121,#4122,#4123,#4124));
#989=EDGE_LOOP('',(#4125,#4126,#4127,#4128));
#990=EDGE_LOOP('',(#4129,#4130,#4131,#4132));
#991=EDGE_LOOP('',(#4133,#4134,#4135,#4136,#4137));
#992=EDGE_LOOP('',(#4138,#4139,#4140,#4141));
#993=EDGE_LOOP('',(#4142,#4143,#4144,#4145));
#994=EDGE_LOOP('',(#4146,#4147,#4148,#4149));
#995=EDGE_LOOP('',(#4150,#4151,#4152,#4153));
#996=EDGE_LOOP('',(#4154,#4155,#4156,#4157));
#997=EDGE_LOOP('',(#4158,#4159,#4160,#4161,#4162));
#998=EDGE_LOOP('',(#4163,#4164,#4165,#4166));
#999=EDGE_LOOP('',(#4167,#4168,#4169,#4170));
#1000=EDGE_LOOP('',(#4171,#4172,#4173,#4174));
#1001=EDGE_LOOP('',(#4175,#4176,#4177,#4178));
#1002=EDGE_LOOP('',(#4179,#4180,#4181,#4182));
#1003=EDGE_LOOP('',(#4183,#4184,#4185,#4186));
#1004=EDGE_LOOP('',(#4187,#4188,#4189,#4190));
#1005=EDGE_LOOP('',(#4191,#4192,#4193,#4194));
#1006=EDGE_LOOP('',(#4195,#4196,#4197,#4198,#4199,#4200,#4201,#4202));
#1007=EDGE_LOOP('',(#4203));
#1008=EDGE_LOOP('',(#4204,#4205,#4206,#4207));
#1009=EDGE_LOOP('',(#4208,#4209,#4210,#4211));
#1010=EDGE_LOOP('',(#4212,#4213,#4214,#4215));
#1011=EDGE_LOOP('',(#4216,#4217,#4218,#4219));
#1012=EDGE_LOOP('',(#4220,#4221,#4222,#4223));
#1013=EDGE_LOOP('',(#4224,#4225,#4226,#4227));
#1014=EDGE_LOOP('',(#4228,#4229,#4230,#4231));
#1015=EDGE_LOOP('',(#4232,#4233,#4234,#4235,#4236,#4237,#4238,#4239));
#1016=EDGE_LOOP('',(#4240));
#1017=EDGE_LOOP('',(#4241,#4242,#4243,#4244));
#1018=EDGE_LOOP('',(#4245,#4246,#4247,#4248));
#1019=EDGE_LOOP('',(#4249,#4250,#4251,#4252));
#1020=EDGE_LOOP('',(#4253,#4254,#4255,#4256));
#1021=EDGE_LOOP('',(#4257,#4258,#4259,#4260));
#1022=EDGE_LOOP('',(#4261,#4262,#4263,#4264,#4265));
#1023=EDGE_LOOP('',(#4266,#4267,#4268,#4269));
#1024=EDGE_LOOP('',(#4270,#4271,#4272,#4273));
#1025=EDGE_LOOP('',(#4274,#4275,#4276,#4277));
#1026=EDGE_LOOP('',(#4278,#4279,#4280,#4281));
#1027=EDGE_LOOP('',(#4282,#4283,#4284,#4285));
#1028=EDGE_LOOP('',(#4286,#4287,#4288,#4289,#4290));
#1029=EDGE_LOOP('',(#4291,#4292,#4293,#4294));
#1030=EDGE_LOOP('',(#4295,#4296,#4297,#4298));
#1031=EDGE_LOOP('',(#4299,#4300,#4301,#4302));
#1032=EDGE_LOOP('',(#4303,#4304,#4305,#4306));
#1033=EDGE_LOOP('',(#4307,#4308,#4309,#4310));
#1034=EDGE_LOOP('',(#4311,#4312,#4313,#4314));
#1035=EDGE_LOOP('',(#4315));
#1036=EDGE_LOOP('',(#4316));
#1037=EDGE_LOOP('',(#4317));
#1038=EDGE_LOOP('',(#4318));
#1039=EDGE_LOOP('',(#4319,#4320,#4321,#4322,#4323,#4324,#4325,#4326,#4327,
#4328,#4329,#4330,#4331,#4332,#4333,#4334,#4335,#4336,#4337,#4338,#4339,
#4340,#4341,#4342,#4343,#4344,#4345,#4346,#4347,#4348,#4349,#4350,#4351,
#4352,#4353,#4354,#4355,#4356,#4357,#4358,#4359,#4360,#4361,#4362,#4363,
#4364,#4365,#4366,#4367,#4368,#4369,#4370,#4371,#4372,#4373,#4374,#4375,
#4376,#4377,#4378,#4379,#4380,#4381,#4382,#4383,#4384,#4385,#4386,#4387,
#4388,#4389,#4390,#4391,#4392,#4393,#4394,#4395,#4396,#4397,#4398));
#1040=EDGE_LOOP('',(#4399));
#1041=EDGE_LOOP('',(#4400,#4401,#4402,#4403,#4404,#4405,#4406,#4407,#4408,
#4409,#4410,#4411,#4412,#4413,#4414,#4415,#4416,#4417,#4418,#4419,#4420,
#4421,#4422,#4423,#4424,#4425,#4426,#4427,#4428,#4429,#4430,#4431,#4432,
#4433,#4434,#4435,#4436,#4437,#4438,#4439,#4440,#4441,#4442,#4443,#4444,
#4445,#4446,#4447,#4448,#4449,#4450,#4451,#4452,#4453,#4454,#4455,#4456,
#4457,#4458,#4459,#4460,#4461,#4462,#4463,#4464,#4465,#4466,#4467,#4468,
#4469,#4470,#4471,#4472,#4473,#4474,#4475,#4476,#4477,#4478,#4479));
#1042=EDGE_LOOP('',(#4480));
#1043=EDGE_LOOP('',(#4481,#4482,#4483,#4484));
#1044=EDGE_LOOP('',(#4485,#4486,#4487,#4488));
#1045=EDGE_LOOP('',(#4489,#4490,#4491,#4492));
#1046=EDGE_LOOP('',(#4493,#4494,#4495,#4496));
#1047=EDGE_LOOP('',(#4497,#4498,#4499,#4500));
#1048=EDGE_LOOP('',(#4501,#4502,#4503,#4504));
#1049=EDGE_LOOP('',(#4505,#4506,#4507,#4508));
#1050=EDGE_LOOP('',(#4509,#4510,#4511,#4512));
#1051=EDGE_LOOP('',(#4513,#4514,#4515,#4516));
#1052=EDGE_LOOP('',(#4517,#4518,#4519,#4520));
#1053=EDGE_LOOP('',(#4521,#4522,#4523,#4524));
#1054=EDGE_LOOP('',(#4525,#4526,#4527,#4528));
#1055=EDGE_LOOP('',(#4529,#4530,#4531,#4532));
#1056=EDGE_LOOP('',(#4533,#4534,#4535,#4536));
#1057=EDGE_LOOP('',(#4537,#4538,#4539,#4540));
#1058=EDGE_LOOP('',(#4541,#4542,#4543,#4544));
#1059=EDGE_LOOP('',(#4545,#4546,#4547,#4548));
#1060=EDGE_LOOP('',(#4549,#4550,#4551,#4552));
#1061=EDGE_LOOP('',(#4553,#4554,#4555,#4556));
#1062=EDGE_LOOP('',(#4557,#4558,#4559,#4560));
#1063=EDGE_LOOP('',(#4561,#4562,#4563,#4564));
#1064=EDGE_LOOP('',(#4565,#4566,#4567,#4568));
#1065=EDGE_LOOP('',(#4569,#4570,#4571,#4572));
#1066=EDGE_LOOP('',(#4573,#4574,#4575,#4576));
#1067=EDGE_LOOP('',(#4577,#4578,#4579,#4580));
#1068=EDGE_LOOP('',(#4581,#4582,#4583,#4584));
#1069=EDGE_LOOP('',(#4585,#4586,#4587,#4588));
#1070=EDGE_LOOP('',(#4589,#4590,#4591,#4592));
#1071=EDGE_LOOP('',(#4593,#4594,#4595,#4596));
#1072=EDGE_LOOP('',(#4597,#4598,#4599,#4600));
#1073=EDGE_LOOP('',(#4601,#4602,#4603,#4604));
#1074=EDGE_LOOP('',(#4605,#4606,#4607,#4608));
#1075=EDGE_LOOP('',(#4609,#4610,#4611,#4612));
#1076=EDGE_LOOP('',(#4613,#4614,#4615,#4616));
#1077=EDGE_LOOP('',(#4617,#4618,#4619,#4620));
#1078=EDGE_LOOP('',(#4621,#4622,#4623,#4624));
#1079=EDGE_LOOP('',(#4625,#4626,#4627,#4628));
#1080=EDGE_LOOP('',(#4629,#4630,#4631,#4632));
#1081=EDGE_LOOP('',(#4633,#4634,#4635,#4636));
#1082=EDGE_LOOP('',(#4637,#4638,#4639,#4640));
#1083=EDGE_LOOP('',(#4641,#4642,#4643,#4644));
#1084=EDGE_LOOP('',(#4645,#4646,#4647,#4648));
#1085=EDGE_LOOP('',(#4649,#4650,#4651,#4652));
#1086=EDGE_LOOP('',(#4653,#4654,#4655,#4656));
#1087=EDGE_LOOP('',(#4657,#4658,#4659,#4660));
#1088=EDGE_LOOP('',(#4661,#4662,#4663,#4664));
#1089=EDGE_LOOP('',(#4665,#4666,#4667,#4668));
#1090=EDGE_LOOP('',(#4669,#4670,#4671,#4672));
#1091=EDGE_LOOP('',(#4673,#4674,#4675,#4676));
#1092=EDGE_LOOP('',(#4677,#4678,#4679,#4680));
#1093=EDGE_LOOP('',(#4681,#4682,#4683,#4684));
#1094=EDGE_LOOP('',(#4685,#4686,#4687,#4688));
#1095=EDGE_LOOP('',(#4689,#4690,#4691,#4692));
#1096=EDGE_LOOP('',(#4693,#4694,#4695,#4696));
#1097=EDGE_LOOP('',(#4697,#4698,#4699,#4700));
#1098=EDGE_LOOP('',(#4701,#4702,#4703,#4704));
#1099=EDGE_LOOP('',(#4705,#4706,#4707,#4708));
#1100=EDGE_LOOP('',(#4709,#4710,#4711,#4712));
#1101=EDGE_LOOP('',(#4713,#4714,#4715,#4716));
#1102=EDGE_LOOP('',(#4717,#4718,#4719,#4720));
#1103=EDGE_LOOP('',(#4721,#4722,#4723,#4724));
#1104=EDGE_LOOP('',(#4725,#4726,#4727,#4728));
#1105=EDGE_LOOP('',(#4729,#4730,#4731,#4732));
#1106=EDGE_LOOP('',(#4733,#4734,#4735,#4736));
#1107=EDGE_LOOP('',(#4737,#4738,#4739,#4740));
#1108=EDGE_LOOP('',(#4741,#4742,#4743,#4744));
#1109=EDGE_LOOP('',(#4745,#4746,#4747,#4748));
#1110=EDGE_LOOP('',(#4749,#4750,#4751,#4752));
#1111=EDGE_LOOP('',(#4753,#4754,#4755,#4756));
#1112=EDGE_LOOP('',(#4757,#4758,#4759,#4760));
#1113=EDGE_LOOP('',(#4761,#4762,#4763,#4764));
#1114=EDGE_LOOP('',(#4765,#4766,#4767,#4768));
#1115=EDGE_LOOP('',(#4769,#4770,#4771,#4772));
#1116=EDGE_LOOP('',(#4773,#4774,#4775,#4776));
#1117=EDGE_LOOP('',(#4777,#4778,#4779,#4780));
#1118=EDGE_LOOP('',(#4781,#4782,#4783,#4784));
#1119=EDGE_LOOP('',(#4785,#4786,#4787,#4788));
#1120=EDGE_LOOP('',(#4789,#4790,#4791,#4792));
#1121=EDGE_LOOP('',(#4793,#4794,#4795,#4796));
#1122=EDGE_LOOP('',(#4797));
#1123=EDGE_LOOP('',(#4798));
#1124=EDGE_LOOP('',(#4799));
#1125=EDGE_LOOP('',(#4800));
#1126=EDGE_LOOP('',(#4801,#4802,#4803,#4804));
#1127=EDGE_LOOP('',(#4805,#4806,#4807,#4808));
#1128=EDGE_LOOP('',(#4809,#4810,#4811,#4812));
#1129=EDGE_LOOP('',(#4813));
#1130=EDGE_LOOP('',(#4814));
#1131=EDGE_LOOP('',(#4815,#4816,#4817,#4818));
#1132=EDGE_LOOP('',(#4819));
#1133=EDGE_LOOP('',(#4820));
#1134=EDGE_LOOP('',(#4821,#4822,#4823,#4824));
#1135=EDGE_LOOP('',(#4825,#4826,#4827,#4828));
#1136=EDGE_LOOP('',(#4829,#4830,#4831,#4832));
#1137=EDGE_LOOP('',(#4833,#4834,#4835,#4836));
#1138=EDGE_LOOP('',(#4837,#4838,#4839,#4840,#4841,#4842,#4843,#4844));
#1139=EDGE_LOOP('',(#4845,#4846,#4847,#4848));
#1140=EDGE_LOOP('',(#4849,#4850,#4851,#4852));
#1141=EDGE_LOOP('',(#4853,#4854,#4855,#4856));
#1142=EDGE_LOOP('',(#4857,#4858,#4859,#4860));
#1143=EDGE_LOOP('',(#4861));
#1144=EDGE_LOOP('',(#4862));
#1145=EDGE_LOOP('',(#4863));
#1146=EDGE_LOOP('',(#4864,#4865,#4866,#4867,#4868,#4869));
#1147=EDGE_LOOP('',(#4870));
#1148=EDGE_LOOP('',(#4871));
#1149=EDGE_LOOP('',(#4872));
#1150=EDGE_LOOP('',(#4873,#4874,#4875,#4876,#4877));
#1151=EDGE_LOOP('',(#4878,#4879,#4880,#4881,#4882));
#1152=EDGE_LOOP('',(#4883,#4884,#4885,#4886,#4887));
#1153=EDGE_LOOP('',(#4888,#4889,#4890,#4891,#4892));
#1154=EDGE_LOOP('',(#4893,#4894,#4895,#4896,#4897));
#1155=EDGE_LOOP('',(#4898,#4899,#4900,#4901,#4902));
#1156=EDGE_LOOP('',(#4903,#4904,#4905));
#1157=EDGE_LOOP('',(#4906,#4907,#4908));
#1158=EDGE_LOOP('',(#4909,#4910,#4911));
#1159=EDGE_LOOP('',(#4912,#4913,#4914));
#1160=EDGE_LOOP('',(#4915,#4916,#4917));
#1161=EDGE_LOOP('',(#4918,#4919,#4920));
#1162=EDGE_LOOP('',(#4921,#4922,#4923,#4924,#4925,#4926,#4927,#4928));
#1163=EDGE_LOOP('',(#4929,#4930,#4931,#4932));
#1164=EDGE_LOOP('',(#4933,#4934,#4935,#4936));
#1165=EDGE_LOOP('',(#4937,#4938,#4939,#4940));
#1166=EDGE_LOOP('',(#4941,#4942,#4943,#4944));
#1167=EDGE_LOOP('',(#4945));
#1168=EDGE_LOOP('',(#4946));
#1169=EDGE_LOOP('',(#4947));
#1170=EDGE_LOOP('',(#4948,#4949,#4950,#4951,#4952,#4953));
#1171=EDGE_LOOP('',(#4954));
#1172=EDGE_LOOP('',(#4955));
#1173=EDGE_LOOP('',(#4956));
#1174=EDGE_LOOP('',(#4957,#4958,#4959,#4960,#4961));
#1175=EDGE_LOOP('',(#4962,#4963,#4964,#4965,#4966));
#1176=EDGE_LOOP('',(#4967,#4968,#4969,#4970,#4971));
#1177=EDGE_LOOP('',(#4972,#4973,#4974,#4975,#4976));
#1178=EDGE_LOOP('',(#4977,#4978,#4979,#4980,#4981));
#1179=EDGE_LOOP('',(#4982,#4983,#4984,#4985,#4986));
#1180=EDGE_LOOP('',(#4987,#4988,#4989));
#1181=EDGE_LOOP('',(#4990,#4991,#4992));
#1182=EDGE_LOOP('',(#4993,#4994,#4995));
#1183=EDGE_LOOP('',(#4996,#4997,#4998));
#1184=EDGE_LOOP('',(#4999,#5000,#5001));
#1185=EDGE_LOOP('',(#5002,#5003,#5004));
#1186=EDGE_LOOP('',(#5005,#5006,#5007,#5008,#5009,#5010,#5011,#5012));
#1187=EDGE_LOOP('',(#5013,#5014,#5015,#5016));
#1188=EDGE_LOOP('',(#5017,#5018,#5019,#5020));
#1189=EDGE_LOOP('',(#5021,#5022,#5023,#5024));
#1190=EDGE_LOOP('',(#5025,#5026,#5027,#5028));
#1191=EDGE_LOOP('',(#5029));
#1192=EDGE_LOOP('',(#5030));
#1193=EDGE_LOOP('',(#5031));
#1194=EDGE_LOOP('',(#5032,#5033,#5034,#5035,#5036,#5037));
#1195=EDGE_LOOP('',(#5038));
#1196=EDGE_LOOP('',(#5039));
#1197=EDGE_LOOP('',(#5040));
#1198=EDGE_LOOP('',(#5041,#5042,#5043,#5044,#5045));
#1199=EDGE_LOOP('',(#5046,#5047,#5048,#5049,#5050));
#1200=EDGE_LOOP('',(#5051,#5052,#5053,#5054,#5055));
#1201=EDGE_LOOP('',(#5056,#5057,#5058,#5059,#5060));
#1202=EDGE_LOOP('',(#5061,#5062,#5063,#5064,#5065));
#1203=EDGE_LOOP('',(#5066,#5067,#5068,#5069,#5070));
#1204=EDGE_LOOP('',(#5071,#5072,#5073));
#1205=EDGE_LOOP('',(#5074,#5075,#5076));
#1206=EDGE_LOOP('',(#5077,#5078,#5079));
#1207=EDGE_LOOP('',(#5080,#5081,#5082));
#1208=EDGE_LOOP('',(#5083,#5084,#5085));
#1209=EDGE_LOOP('',(#5086,#5087,#5088));
#1210=EDGE_LOOP('',(#5089,#5090,#5091,#5092,#5093,#5094,#5095,#5096));
#1211=EDGE_LOOP('',(#5097,#5098,#5099,#5100));
#1212=EDGE_LOOP('',(#5101,#5102,#5103,#5104));
#1213=EDGE_LOOP('',(#5105,#5106,#5107,#5108));
#1214=EDGE_LOOP('',(#5109,#5110,#5111,#5112));
#1215=EDGE_LOOP('',(#5113));
#1216=EDGE_LOOP('',(#5114));
#1217=EDGE_LOOP('',(#5115));
#1218=EDGE_LOOP('',(#5116,#5117,#5118,#5119,#5120,#5121));
#1219=EDGE_LOOP('',(#5122));
#1220=EDGE_LOOP('',(#5123));
#1221=EDGE_LOOP('',(#5124));
#1222=EDGE_LOOP('',(#5125,#5126,#5127,#5128,#5129));
#1223=EDGE_LOOP('',(#5130,#5131,#5132,#5133,#5134));
#1224=EDGE_LOOP('',(#5135,#5136,#5137,#5138,#5139));
#1225=EDGE_LOOP('',(#5140,#5141,#5142,#5143,#5144));
#1226=EDGE_LOOP('',(#5145,#5146,#5147,#5148,#5149));
#1227=EDGE_LOOP('',(#5150,#5151,#5152,#5153,#5154));
#1228=EDGE_LOOP('',(#5155,#5156,#5157));
#1229=EDGE_LOOP('',(#5158,#5159,#5160));
#1230=EDGE_LOOP('',(#5161,#5162,#5163));
#1231=EDGE_LOOP('',(#5164,#5165,#5166));
#1232=EDGE_LOOP('',(#5167,#5168,#5169));
#1233=EDGE_LOOP('',(#5170,#5171,#5172));
#1234=LINE('',#7771,#1691);
#1235=LINE('',#7777,#1692);
#1236=LINE('',#7783,#1693);
#1237=LINE('',#7789,#1694);
#1238=LINE('',#7795,#1695);
#1239=LINE('',#7801,#1696);
#1240=LINE('',#7807,#1697);
#1241=LINE('',#7814,#1698);
#1242=LINE('',#7817,#1699);
#1243=LINE('',#7820,#1700);
#1244=LINE('',#7822,#1701);
#1245=LINE('',#7823,#1702);
#1246=LINE('',#7828,#1703);
#1247=LINE('',#7832,#1704);
#1248=LINE('',#7834,#1705);
#1249=LINE('',#7835,#1706);
#1250=LINE('',#7840,#1707);
#1251=LINE('',#7844,#1708);
#1252=LINE('',#7846,#1709);
#1253=LINE('',#7847,#1710);
#1254=LINE('',#7852,#1711);
#1255=LINE('',#7855,#1712);
#1256=LINE('',#7856,#1713);
#1257=LINE('',#7863,#1714);
#1258=LINE('',#7869,#1715);
#1259=LINE('',#7875,#1716);
#1260=LINE('',#7881,#1717);
#1261=LINE('',#7888,#1718);
#1262=LINE('',#7891,#1719);
#1263=LINE('',#7896,#1720);
#1264=LINE('',#7902,#1721);
#1265=LINE('',#7908,#1722);
#1266=LINE('',#7912,#1723);
#1267=LINE('',#7914,#1724);
#1268=LINE('',#7915,#1725);
#1269=LINE('',#7920,#1726);
#1270=LINE('',#7924,#1727);
#1271=LINE('',#7926,#1728);
#1272=LINE('',#7927,#1729);
#1273=LINE('',#7932,#1730);
#1274=LINE('',#7936,#1731);
#1275=LINE('',#7938,#1732);
#1276=LINE('',#7939,#1733);
#1277=LINE('',#7944,#1734);
#1278=LINE('',#7947,#1735);
#1279=LINE('',#7948,#1736);
#1280=LINE('',#7954,#1737);
#1281=LINE('',#7956,#1738);
#1282=LINE('',#7958,#1739);
#1283=LINE('',#7959,#1740);
#1284=LINE('',#7962,#1741);
#1285=LINE('',#7964,#1742);
#1286=LINE('',#7965,#1743);
#1287=LINE('',#7968,#1744);
#1288=LINE('',#7970,#1745);
#1289=LINE('',#7971,#1746);
#1290=LINE('',#7974,#1747);
#1291=LINE('',#7976,#1748);
#1292=LINE('',#7977,#1749);
#1293=LINE('',#7980,#1750);
#1294=LINE('',#7982,#1751);
#1295=LINE('',#7983,#1752);
#1296=LINE('',#7985,#1753);
#1297=LINE('',#7986,#1754);
#1298=LINE('',#7992,#1755);
#1299=LINE('',#7994,#1756);
#1300=LINE('',#7996,#1757);
#1301=LINE('',#7997,#1758);
#1302=LINE('',#8000,#1759);
#1303=LINE('',#8002,#1760);
#1304=LINE('',#8003,#1761);
#1305=LINE('',#8006,#1762);
#1306=LINE('',#8008,#1763);
#1307=LINE('',#8009,#1764);
#1308=LINE('',#8012,#1765);
#1309=LINE('',#8014,#1766);
#1310=LINE('',#8015,#1767);
#1311=LINE('',#8018,#1768);
#1312=LINE('',#8020,#1769);
#1313=LINE('',#8021,#1770);
#1314=LINE('',#8023,#1771);
#1315=LINE('',#8024,#1772);
#1316=LINE('',#8030,#1773);
#1317=LINE('',#8032,#1774);
#1318=LINE('',#8034,#1775);
#1319=LINE('',#8035,#1776);
#1320=LINE('',#8038,#1777);
#1321=LINE('',#8040,#1778);
#1322=LINE('',#8041,#1779);
#1323=LINE('',#8044,#1780);
#1324=LINE('',#8046,#1781);
#1325=LINE('',#8047,#1782);
#1326=LINE('',#8050,#1783);
#1327=LINE('',#8052,#1784);
#1328=LINE('',#8053,#1785);
#1329=LINE('',#8056,#1786);
#1330=LINE('',#8058,#1787);
#1331=LINE('',#8059,#1788);
#1332=LINE('',#8061,#1789);
#1333=LINE('',#8062,#1790);
#1334=LINE('',#8070,#1791);
#1335=LINE('',#8077,#1792);
#1336=LINE('',#8080,#1793);
#1337=LINE('',#8085,#1794);
#1338=LINE('',#8091,#1795);
#1339=LINE('',#8097,#1796);
#1340=LINE('',#8104,#1797);
#1341=LINE('',#8106,#1798);
#1342=LINE('',#8110,#1799);
#1343=LINE('',#8114,#1800);
#1344=LINE('',#8116,#1801);
#1345=LINE('',#8118,#1802);
#1346=LINE('',#8120,#1803);
#1347=LINE('',#8122,#1804);
#1348=LINE('',#8124,#1805);
#1349=LINE('',#8128,#1806);
#1350=LINE('',#8130,#1807);
#1351=LINE('',#8132,#1808);
#1352=LINE('',#8134,#1809);
#1353=LINE('',#8136,#1810);
#1354=LINE('',#8138,#1811);
#1355=LINE('',#8140,#1812);
#1356=LINE('',#8141,#1813);
#1357=LINE('',#8146,#1814);
#1358=LINE('',#8148,#1815);
#1359=LINE('',#8150,#1816);
#1360=LINE('',#8152,#1817);
#1361=LINE('',#8156,#1818);
#1362=LINE('',#8157,#1819);
#1363=LINE('',#8160,#1820);
#1364=LINE('',#8162,#1821);
#1365=LINE('',#8164,#1822);
#1366=LINE('',#8167,#1823);
#1367=LINE('',#8170,#1824);
#1368=LINE('',#8172,#1825);
#1369=LINE('',#8174,#1826);
#1370=LINE('',#8176,#1827);
#1371=LINE('',#8181,#1828);
#1372=LINE('',#8183,#1829);
#1373=LINE('',#8185,#1830);
#1374=LINE('',#8187,#1831);
#1375=LINE('',#8189,#1832);
#1376=LINE('',#8191,#1833);
#1377=LINE('',#8193,#1834);
#1378=LINE('',#8195,#1835);
#1379=LINE('',#8197,#1836);
#1380=LINE('',#8201,#1837);
#1381=LINE('',#8203,#1838);
#1382=LINE('',#8205,#1839);
#1383=LINE('',#8207,#1840);
#1384=LINE('',#8209,#1841);
#1385=LINE('',#8211,#1842);
#1386=LINE('',#8215,#1843);
#1387=LINE('',#8218,#1844);
#1388=LINE('',#8221,#1845);
#1389=LINE('',#8223,#1846);
#1390=LINE('',#8225,#1847);
#1391=LINE('',#8227,#1848);
#1392=LINE('',#8231,#1849);
#1393=LINE('',#8233,#1850);
#1394=LINE('',#8235,#1851);
#1395=LINE('',#8238,#1852);
#1396=LINE('',#8240,#1853);
#1397=LINE('',#8242,#1854);
#1398=LINE('',#8246,#1855);
#1399=LINE('',#8248,#1856);
#1400=LINE('',#8250,#1857);
#1401=LINE('',#8251,#1858);
#1402=LINE('',#8253,#1859);
#1403=LINE('',#8254,#1860);
#1404=LINE('',#8256,#1861);
#1405=LINE('',#8258,#1862);
#1406=LINE('',#8260,#1863);
#1407=LINE('',#8262,#1864);
#1408=LINE('',#8264,#1865);
#1409=LINE('',#8266,#1866);
#1410=LINE('',#8268,#1867);
#1411=LINE('',#8270,#1868);
#1412=LINE('',#8272,#1869);
#1413=LINE('',#8274,#1870);
#1414=LINE('',#8276,#1871);
#1415=LINE('',#8278,#1872);
#1416=LINE('',#8280,#1873);
#1417=LINE('',#8282,#1874);
#1418=LINE('',#8284,#1875);
#1419=LINE('',#8286,#1876);
#1420=LINE('',#8288,#1877);
#1421=LINE('',#8290,#1878);
#1422=LINE('',#8294,#1879);
#1423=LINE('',#8296,#1880);
#1424=LINE('',#8297,#1881);
#1425=LINE('',#8300,#1882);
#1426=LINE('',#8301,#1883);
#1427=LINE('',#8304,#1884);
#1428=LINE('',#8305,#1885);
#1429=LINE('',#8308,#1886);
#1430=LINE('',#8309,#1887);
#1431=LINE('',#8315,#1888);
#1432=LINE('',#8317,#1889);
#1433=LINE('',#8318,#1890);
#1434=LINE('',#8321,#1891);
#1435=LINE('',#8322,#1892);
#1436=LINE('',#8325,#1893);
#1437=LINE('',#8326,#1894);
#1438=LINE('',#8330,#1895);
#1439=LINE('',#8332,#1896);
#1440=LINE('',#8336,#1897);
#1441=LINE('',#8339,#1898);
#1442=LINE('',#8342,#1899);
#1443=LINE('',#8343,#1900);
#1444=LINE('',#8346,#1901);
#1445=LINE('',#8347,#1902);
#1446=LINE('',#8350,#1903);
#1447=LINE('',#8351,#1904);
#1448=LINE('',#8354,#1905);
#1449=LINE('',#8355,#1906);
#1450=LINE('',#8359,#1907);
#1451=LINE('',#8362,#1908);
#1452=LINE('',#8363,#1909);
#1453=LINE('',#8365,#1910);
#1454=LINE('',#8369,#1911);
#1455=LINE('',#8370,#1912);
#1456=LINE('',#8373,#1913);
#1457=LINE('',#8374,#1914);
#1458=LINE('',#8378,#1915);
#1459=LINE('',#8381,#1916);
#1460=LINE('',#8382,#1917);
#1461=LINE('',#8385,#1918);
#1462=LINE('',#8386,#1919);
#1463=LINE('',#8389,#1920);
#1464=LINE('',#8390,#1921);
#1465=LINE('',#8392,#1922);
#1466=LINE('',#8396,#1923);
#1467=LINE('',#8398,#1924);
#1468=LINE('',#8399,#1925);
#1469=LINE('',#8402,#1926);
#1470=LINE('',#8403,#1927);
#1471=LINE('',#8407,#1928);
#1472=LINE('',#8410,#1929);
#1473=LINE('',#8411,#1930);
#1474=LINE('',#8413,#1931);
#1475=LINE('',#8417,#1932);
#1476=LINE('',#8419,#1933);
#1477=LINE('',#8420,#1934);
#1478=LINE('',#8423,#1935);
#1479=LINE('',#8424,#1936);
#1480=LINE('',#8427,#1937);
#1481=LINE('',#8428,#1938);
#1482=LINE('',#8432,#1939);
#1483=LINE('',#8434,#1940);
#1484=LINE('',#8441,#1941);
#1485=LINE('',#8447,#1942);
#1486=LINE('',#8453,#1943);
#1487=LINE('',#8459,#1944);
#1488=LINE('',#8465,#1945);
#1489=LINE('',#8472,#1946);
#1490=LINE('',#8475,#1947);
#1491=LINE('',#10600,#1948);
#1492=LINE('',#10601,#1949);
#1493=LINE('',#10603,#1950);
#1494=LINE('',#10650,#1951);
#1495=LINE('',#10652,#1952);
#1496=LINE('',#10699,#1953);
#1497=LINE('',#10701,#1954);
#1498=LINE('',#10748,#1955);
#1499=LINE('',#10750,#1956);
#1500=LINE('',#10797,#1957);
#1501=LINE('',#10799,#1958);
#1502=LINE('',#10846,#1959);
#1503=LINE('',#10848,#1960);
#1504=LINE('',#10895,#1961);
#1505=LINE('',#10897,#1962);
#1506=LINE('',#10944,#1963);
#1507=LINE('',#10946,#1964);
#1508=LINE('',#10993,#1965);
#1509=LINE('',#10995,#1966);
#1510=LINE('',#11042,#1967);
#1511=LINE('',#11044,#1968);
#1512=LINE('',#11091,#1969);
#1513=LINE('',#11093,#1970);
#1514=LINE('',#11140,#1971);
#1515=LINE('',#11142,#1972);
#1516=LINE('',#11189,#1973);
#1517=LINE('',#11191,#1974);
#1518=LINE('',#11238,#1975);
#1519=LINE('',#11240,#1976);
#1520=LINE('',#11287,#1977);
#1521=LINE('',#11289,#1978);
#1522=LINE('',#11336,#1979);
#1523=LINE('',#11338,#1980);
#1524=LINE('',#11385,#1981);
#1525=LINE('',#11387,#1982);
#1526=LINE('',#11480,#1983);
#1527=LINE('',#11482,#1984);
#1528=LINE('',#11529,#1985);
#1529=LINE('',#11531,#1986);
#1530=LINE('',#11578,#1987);
#1531=LINE('',#11580,#1988);
#1532=LINE('',#11627,#1989);
#1533=LINE('',#11629,#1990);
#1534=LINE('',#11676,#1991);
#1535=LINE('',#11678,#1992);
#1536=LINE('',#11725,#1993);
#1537=LINE('',#11727,#1994);
#1538=LINE('',#11774,#1995);
#1539=LINE('',#11776,#1996);
#1540=LINE('',#11823,#1997);
#1541=LINE('',#11825,#1998);
#1542=LINE('',#11872,#1999);
#1543=LINE('',#11874,#2000);
#1544=LINE('',#11921,#2001);
#1545=LINE('',#11923,#2002);
#1546=LINE('',#11970,#2003);
#1547=LINE('',#11972,#2004);
#1548=LINE('',#12019,#2005);
#1549=LINE('',#12021,#2006);
#1550=LINE('',#12068,#2007);
#1551=LINE('',#12070,#2008);
#1552=LINE('',#12117,#2009);
#1553=LINE('',#12119,#2010);
#1554=LINE('',#12166,#2011);
#1555=LINE('',#12168,#2012);
#1556=LINE('',#12215,#2013);
#1557=LINE('',#12217,#2014);
#1558=LINE('',#12264,#2015);
#1559=LINE('',#12266,#2016);
#1560=LINE('',#12313,#2017);
#1561=LINE('',#12315,#2018);
#1562=LINE('',#12362,#2019);
#1563=LINE('',#12364,#2020);
#1564=LINE('',#12411,#2021);
#1565=LINE('',#12413,#2022);
#1566=LINE('',#12460,#2023);
#1567=LINE('',#12462,#2024);
#1568=LINE('',#12509,#2025);
#1569=LINE('',#12518,#2026);
#1570=LINE('',#12524,#2027);
#1571=LINE('',#12531,#2028);
#1572=LINE('',#12534,#2029);
#1573=LINE('',#12540,#2030);
#1574=LINE('',#12543,#2031);
#1575=LINE('',#12545,#2032);
#1576=LINE('',#12546,#2033);
#1577=LINE('',#12548,#2034);
#1578=LINE('',#12550,#2035);
#1579=LINE('',#12556,#2036);
#1580=LINE('',#12578,#2037);
#1581=LINE('',#12581,#2038);
#1582=LINE('',#12586,#2039);
#1583=LINE('',#12594,#2040);
#1584=LINE('',#12596,#2041);
#1585=LINE('',#12598,#2042);
#1586=LINE('',#12600,#2043);
#1587=LINE('',#12602,#2044);
#1588=LINE('',#12603,#2045);
#1589=LINE('',#12608,#2046);
#1590=LINE('',#12610,#2047);
#1591=LINE('',#12611,#2048);
#1592=LINE('',#12612,#2049);
#1593=LINE('',#12614,#2050);
#1594=LINE('',#12616,#2051);
#1595=LINE('',#12617,#2052);
#1596=LINE('',#12619,#2053);
#1597=LINE('',#12621,#2054);
#1598=LINE('',#12622,#2055);
#1599=LINE('',#12624,#2056);
#1600=LINE('',#12626,#2057);
#1601=LINE('',#12627,#2058);
#1602=LINE('',#12629,#2059);
#1603=LINE('',#12631,#2060);
#1604=LINE('',#12632,#2061);
#1605=LINE('',#12634,#2062);
#1606=LINE('',#12635,#2063);
#1607=LINE('',#12646,#2064);
#1608=LINE('',#12668,#2065);
#1609=LINE('',#12671,#2066);
#1610=LINE('',#12676,#2067);
#1611=LINE('',#12684,#2068);
#1612=LINE('',#12686,#2069);
#1613=LINE('',#12688,#2070);
#1614=LINE('',#12690,#2071);
#1615=LINE('',#12692,#2072);
#1616=LINE('',#12693,#2073);
#1617=LINE('',#12698,#2074);
#1618=LINE('',#12700,#2075);
#1619=LINE('',#12701,#2076);
#1620=LINE('',#12702,#2077);
#1621=LINE('',#12704,#2078);
#1622=LINE('',#12706,#2079);
#1623=LINE('',#12707,#2080);
#1624=LINE('',#12709,#2081);
#1625=LINE('',#12711,#2082);
#1626=LINE('',#12712,#2083);
#1627=LINE('',#12714,#2084);
#1628=LINE('',#12716,#2085);
#1629=LINE('',#12717,#2086);
#1630=LINE('',#12719,#2087);
#1631=LINE('',#12721,#2088);
#1632=LINE('',#12722,#2089);
#1633=LINE('',#12724,#2090);
#1634=LINE('',#12725,#2091);
#1635=LINE('',#12736,#2092);
#1636=LINE('',#12758,#2093);
#1637=LINE('',#12761,#2094);
#1638=LINE('',#12766,#2095);
#1639=LINE('',#12774,#2096);
#1640=LINE('',#12776,#2097);
#1641=LINE('',#12778,#2098);
#1642=LINE('',#12780,#2099);
#1643=LINE('',#12782,#2100);
#1644=LINE('',#12783,#2101);
#1645=LINE('',#12788,#2102);
#1646=LINE('',#12790,#2103);
#1647=LINE('',#12791,#2104);
#1648=LINE('',#12792,#2105);
#1649=LINE('',#12794,#2106);
#1650=LINE('',#12796,#2107);
#1651=LINE('',#12797,#2108);
#1652=LINE('',#12799,#2109);
#1653=LINE('',#12801,#2110);
#1654=LINE('',#12802,#2111);
#1655=LINE('',#12804,#2112);
#1656=LINE('',#12806,#2113);
#1657=LINE('',#12807,#2114);
#1658=LINE('',#12809,#2115);
#1659=LINE('',#12811,#2116);
#1660=LINE('',#12812,#2117);
#1661=LINE('',#12814,#2118);
#1662=LINE('',#12815,#2119);
#1663=LINE('',#12826,#2120);
#1664=LINE('',#12848,#2121);
#1665=LINE('',#12851,#2122);
#1666=LINE('',#12856,#2123);
#1667=LINE('',#12864,#2124);
#1668=LINE('',#12866,#2125);
#1669=LINE('',#12868,#2126);
#1670=LINE('',#12870,#2127);
#1671=LINE('',#12872,#2128);
#1672=LINE('',#12873,#2129);
#1673=LINE('',#12878,#2130);
#1674=LINE('',#12880,#2131);
#1675=LINE('',#12881,#2132);
#1676=LINE('',#12882,#2133);
#1677=LINE('',#12884,#2134);
#1678=LINE('',#12886,#2135);
#1679=LINE('',#12887,#2136);
#1680=LINE('',#12889,#2137);
#1681=LINE('',#12891,#2138);
#1682=LINE('',#12892,#2139);
#1683=LINE('',#12894,#2140);
#1684=LINE('',#12896,#2141);
#1685=LINE('',#12897,#2142);
#1686=LINE('',#12899,#2143);
#1687=LINE('',#12901,#2144);
#1688=LINE('',#12902,#2145);
#1689=LINE('',#12904,#2146);
#1690=LINE('',#12905,#2147);
#1691=VECTOR('',#6230,1.99999999999998);
#1692=VECTOR('',#6237,1.99999999999998);
#1693=VECTOR('',#6244,2.);
#1694=VECTOR('',#6251,2.5);
#1695=VECTOR('',#6258,2.5);
#1696=VECTOR('',#6265,2.5);
#1697=VECTOR('',#6272,2.5);
#1698=VECTOR('',#6279,1000.);
#1699=VECTOR('',#6282,1000.);
#1700=VECTOR('',#6285,1000.);
#1701=VECTOR('',#6286,1000.);
#1702=VECTOR('',#6287,1000.);
#1703=VECTOR('',#6292,1000.);
#1704=VECTOR('',#6297,1000.);
#1705=VECTOR('',#6298,1000.);
#1706=VECTOR('',#6299,1000.);
#1707=VECTOR('',#6304,1000.);
#1708=VECTOR('',#6309,1000.);
#1709=VECTOR('',#6310,1000.);
#1710=VECTOR('',#6311,1000.);
#1711=VECTOR('',#6316,1000.);
#1712=VECTOR('',#6321,1000.);
#1713=VECTOR('',#6322,1000.);
#1714=VECTOR('',#6331,1.99999999999998);
#1715=VECTOR('',#6338,1.99999999999998);
#1716=VECTOR('',#6345,2.5);
#1717=VECTOR('',#6352,2.5);
#1718=VECTOR('',#6359,1000.);
#1719=VECTOR('',#6362,1000.);
#1720=VECTOR('',#6367,2.5);
#1721=VECTOR('',#6374,2.5);
#1722=VECTOR('',#6381,2.);
#1723=VECTOR('',#6386,1000.);
#1724=VECTOR('',#6387,1000.);
#1725=VECTOR('',#6388,1000.);
#1726=VECTOR('',#6393,1000.);
#1727=VECTOR('',#6398,1000.);
#1728=VECTOR('',#6399,1000.);
#1729=VECTOR('',#6400,1000.);
#1730=VECTOR('',#6405,1000.);
#1731=VECTOR('',#6410,1000.);
#1732=VECTOR('',#6411,1000.);
#1733=VECTOR('',#6412,1000.);
#1734=VECTOR('',#6417,1000.);
#1735=VECTOR('',#6422,1000.);
#1736=VECTOR('',#6423,1000.);
#1737=VECTOR('',#6430,1000.);
#1738=VECTOR('',#6431,1000.);
#1739=VECTOR('',#6432,1000.);
#1740=VECTOR('',#6433,1000.);
#1741=VECTOR('',#6436,1000.);
#1742=VECTOR('',#6437,1000.);
#1743=VECTOR('',#6438,1000.);
#1744=VECTOR('',#6441,1000.);
#1745=VECTOR('',#6442,1000.);
#1746=VECTOR('',#6443,1000.);
#1747=VECTOR('',#6446,1000.);
#1748=VECTOR('',#6447,1000.);
#1749=VECTOR('',#6448,1000.);
#1750=VECTOR('',#6451,1000.);
#1751=VECTOR('',#6452,1000.);
#1752=VECTOR('',#6453,1000.);
#1753=VECTOR('',#6456,1000.);
#1754=VECTOR('',#6457,1000.);
#1755=VECTOR('',#6464,1000.);
#1756=VECTOR('',#6465,1000.);
#1757=VECTOR('',#6466,1000.);
#1758=VECTOR('',#6467,1000.);
#1759=VECTOR('',#6470,1000.);
#1760=VECTOR('',#6471,1000.);
#1761=VECTOR('',#6472,1000.);
#1762=VECTOR('',#6475,1000.);
#1763=VECTOR('',#6476,1000.);
#1764=VECTOR('',#6477,1000.);
#1765=VECTOR('',#6480,1000.);
#1766=VECTOR('',#6481,1000.);
#1767=VECTOR('',#6482,1000.);
#1768=VECTOR('',#6485,1000.);
#1769=VECTOR('',#6486,1000.);
#1770=VECTOR('',#6487,1000.);
#1771=VECTOR('',#6490,1000.);
#1772=VECTOR('',#6491,1000.);
#1773=VECTOR('',#6498,1000.);
#1774=VECTOR('',#6499,1000.);
#1775=VECTOR('',#6500,1000.);
#1776=VECTOR('',#6501,1000.);
#1777=VECTOR('',#6504,1000.);
#1778=VECTOR('',#6505,1000.);
#1779=VECTOR('',#6506,1000.);
#1780=VECTOR('',#6509,1000.);
#1781=VECTOR('',#6510,1000.);
#1782=VECTOR('',#6511,1000.);
#1783=VECTOR('',#6514,1000.);
#1784=VECTOR('',#6515,1000.);
#1785=VECTOR('',#6516,1000.);
#1786=VECTOR('',#6519,1000.);
#1787=VECTOR('',#6520,1000.);
#1788=VECTOR('',#6521,1000.);
#1789=VECTOR('',#6524,1000.);
#1790=VECTOR('',#6525,1000.);
#1791=VECTOR('',#6536,3.5);
#1792=VECTOR('',#6543,1000.);
#1793=VECTOR('',#6546,1000.);
#1794=VECTOR('',#6551,3.5);
#1795=VECTOR('',#6558,2.5);
#1796=VECTOR('',#6565,2.5);
#1797=VECTOR('',#6574,1000.);
#1798=VECTOR('',#6575,1000.);
#1799=VECTOR('',#6578,1000.);
#1800=VECTOR('',#6581,1000.);
#1801=VECTOR('',#6582,1000.);
#1802=VECTOR('',#6583,1000.);
#1803=VECTOR('',#6584,1000.);
#1804=VECTOR('',#6585,1000.);
#1805=VECTOR('',#6586,1000.);
#1806=VECTOR('',#6589,1000.);
#1807=VECTOR('',#6590,1000.);
#1808=VECTOR('',#6591,1000.);
#1809=VECTOR('',#6592,1000.);
#1810=VECTOR('',#6593,1000.);
#1811=VECTOR('',#6594,1000.);
#1812=VECTOR('',#6595,1000.);
#1813=VECTOR('',#6596,1000.);
#1814=VECTOR('',#6599,1000.);
#1815=VECTOR('',#6600,1000.);
#1816=VECTOR('',#6601,1000.);
#1817=VECTOR('',#6602,1000.);
#1818=VECTOR('',#6605,1000.);
#1819=VECTOR('',#6606,1000.);
#1820=VECTOR('',#6607,1000.);
#1821=VECTOR('',#6608,1000.);
#1822=VECTOR('',#6609,1000.);
#1823=VECTOR('',#6612,1000.);
#1824=VECTOR('',#6613,1000.);
#1825=VECTOR('',#6614,1000.);
#1826=VECTOR('',#6615,1000.);
#1827=VECTOR('',#6616,1000.);
#1828=VECTOR('',#6621,1000.);
#1829=VECTOR('',#6622,1000.);
#1830=VECTOR('',#6623,1000.);
#1831=VECTOR('',#6624,1000.);
#1832=VECTOR('',#6625,1000.);
#1833=VECTOR('',#6626,1000.);
#1834=VECTOR('',#6627,1000.);
#1835=VECTOR('',#6628,1000.);
#1836=VECTOR('',#6629,1000.);
#1837=VECTOR('',#6632,1000.);
#1838=VECTOR('',#6633,1000.);
#1839=VECTOR('',#6634,1000.);
#1840=VECTOR('',#6635,1000.);
#1841=VECTOR('',#6636,1000.);
#1842=VECTOR('',#6637,1000.);
#1843=VECTOR('',#6640,1000.);
#1844=VECTOR('',#6643,1000.);
#1845=VECTOR('',#6644,1000.);
#1846=VECTOR('',#6645,1000.);
#1847=VECTOR('',#6646,1000.);
#1848=VECTOR('',#6647,1000.);
#1849=VECTOR('',#6650,1000.);
#1850=VECTOR('',#6651,1000.);
#1851=VECTOR('',#6652,1000.);
#1852=VECTOR('',#6655,1000.);
#1853=VECTOR('',#6656,1000.);
#1854=VECTOR('',#6657,1000.);
#1855=VECTOR('',#6660,1000.);
#1856=VECTOR('',#6661,1000.);
#1857=VECTOR('',#6662,1000.);
#1858=VECTOR('',#6663,1000.);
#1859=VECTOR('',#6666,1000.);
#1860=VECTOR('',#6667,1000.);
#1861=VECTOR('',#6670,1000.);
#1862=VECTOR('',#6673,1000.);
#1863=VECTOR('',#6676,1000.);
#1864=VECTOR('',#6679,1000.);
#1865=VECTOR('',#6682,1000.);
#1866=VECTOR('',#6685,1000.);
#1867=VECTOR('',#6688,1000.);
#1868=VECTOR('',#6691,1000.);
#1869=VECTOR('',#6694,1000.);
#1870=VECTOR('',#6697,1000.);
#1871=VECTOR('',#6700,1000.);
#1872=VECTOR('',#6703,1000.);
#1873=VECTOR('',#6706,1000.);
#1874=VECTOR('',#6709,1000.);
#1875=VECTOR('',#6712,1000.);
#1876=VECTOR('',#6715,1000.);
#1877=VECTOR('',#6718,1000.);
#1878=VECTOR('',#6721,1000.);
#1879=VECTOR('',#6726,1000.);
#1880=VECTOR('',#6727,1000.);
#1881=VECTOR('',#6728,1000.);
#1882=VECTOR('',#6731,1000.);
#1883=VECTOR('',#6732,1000.);
#1884=VECTOR('',#6735,1000.);
#1885=VECTOR('',#6736,1000.);
#1886=VECTOR('',#6739,1000.);
#1887=VECTOR('',#6740,1000.);
#1888=VECTOR('',#6749,1000.);
#1889=VECTOR('',#6750,1000.);
#1890=VECTOR('',#6751,1000.);
#1891=VECTOR('',#6754,1000.);
#1892=VECTOR('',#6755,1000.);
#1893=VECTOR('',#6758,1000.);
#1894=VECTOR('',#6759,1000.);
#1895=VECTOR('',#6764,1000.);
#1896=VECTOR('',#6767,1000.);
#1897=VECTOR('',#6772,1000.);
#1898=VECTOR('',#6775,1000.);
#1899=VECTOR('',#6778,1000.);
#1900=VECTOR('',#6779,1000.);
#1901=VECTOR('',#6782,1000.);
#1902=VECTOR('',#6783,1000.);
#1903=VECTOR('',#6786,1000.);
#1904=VECTOR('',#6787,1000.);
#1905=VECTOR('',#6790,1000.);
#1906=VECTOR('',#6791,1000.);
#1907=VECTOR('',#6796,1000.);
#1908=VECTOR('',#6799,1000.);
#1909=VECTOR('',#6800,1000.);
#1910=VECTOR('',#6803,1000.);
#1911=VECTOR('',#6808,1000.);
#1912=VECTOR('',#6809,1000.);
#1913=VECTOR('',#6812,1000.);
#1914=VECTOR('',#6813,1000.);
#1915=VECTOR('',#6818,1000.);
#1916=VECTOR('',#6821,1000.);
#1917=VECTOR('',#6822,1000.);
#1918=VECTOR('',#6825,1000.);
#1919=VECTOR('',#6826,1000.);
#1920=VECTOR('',#6829,1000.);
#1921=VECTOR('',#6830,1000.);
#1922=VECTOR('',#6833,1000.);
#1923=VECTOR('',#6838,1000.);
#1924=VECTOR('',#6839,1000.);
#1925=VECTOR('',#6840,1000.);
#1926=VECTOR('',#6843,1000.);
#1927=VECTOR('',#6844,1000.);
#1928=VECTOR('',#6849,1000.);
#1929=VECTOR('',#6852,1000.);
#1930=VECTOR('',#6853,1000.);
#1931=VECTOR('',#6856,1000.);
#1932=VECTOR('',#6861,1000.);
#1933=VECTOR('',#6862,1000.);
#1934=VECTOR('',#6863,1000.);
#1935=VECTOR('',#6866,1000.);
#1936=VECTOR('',#6867,1000.);
#1937=VECTOR('',#6870,1000.);
#1938=VECTOR('',#6871,1000.);
#1939=VECTOR('',#6876,1000.);
#1940=VECTOR('',#6879,1000.);
#1941=VECTOR('',#6888,7.);
#1942=VECTOR('',#6895,14.);
#1943=VECTOR('',#6902,7.);
#1944=VECTOR('',#6909,14.);
#1945=VECTOR('',#6916,2.5);
#1946=VECTOR('',#6923,1000.);
#1947=VECTOR('',#6926,1000.);
#1948=VECTOR('',#7091,1000.);
#1949=VECTOR('',#7092,1000.);
#1950=VECTOR('',#7095,1000.);
#1951=VECTOR('',#7096,1000.);
#1952=VECTOR('',#7099,1000.);
#1953=VECTOR('',#7100,1000.);
#1954=VECTOR('',#7103,1000.);
#1955=VECTOR('',#7104,1000.);
#1956=VECTOR('',#7107,1000.);
#1957=VECTOR('',#7108,1000.);
#1958=VECTOR('',#7111,1000.);
#1959=VECTOR('',#7112,1000.);
#1960=VECTOR('',#7115,1000.);
#1961=VECTOR('',#7116,1000.);
#1962=VECTOR('',#7119,1000.);
#1963=VECTOR('',#7120,1000.);
#1964=VECTOR('',#7123,1000.);
#1965=VECTOR('',#7124,1000.);
#1966=VECTOR('',#7127,1000.);
#1967=VECTOR('',#7128,1000.);
#1968=VECTOR('',#7131,1000.);
#1969=VECTOR('',#7132,1000.);
#1970=VECTOR('',#7135,1000.);
#1971=VECTOR('',#7136,1000.);
#1972=VECTOR('',#7139,1000.);
#1973=VECTOR('',#7140,1000.);
#1974=VECTOR('',#7143,1000.);
#1975=VECTOR('',#7144,1000.);
#1976=VECTOR('',#7147,1000.);
#1977=VECTOR('',#7148,1000.);
#1978=VECTOR('',#7151,1000.);
#1979=VECTOR('',#7152,1000.);
#1980=VECTOR('',#7155,1000.);
#1981=VECTOR('',#7156,1000.);
#1982=VECTOR('',#7159,1000.);
#1983=VECTOR('',#7160,1000.);
#1984=VECTOR('',#7163,1000.);
#1985=VECTOR('',#7164,1000.);
#1986=VECTOR('',#7167,1000.);
#1987=VECTOR('',#7168,1000.);
#1988=VECTOR('',#7171,1000.);
#1989=VECTOR('',#7172,1000.);
#1990=VECTOR('',#7175,1000.);
#1991=VECTOR('',#7176,1000.);
#1992=VECTOR('',#7179,1000.);
#1993=VECTOR('',#7180,1000.);
#1994=VECTOR('',#7183,1000.);
#1995=VECTOR('',#7184,1000.);
#1996=VECTOR('',#7187,1000.);
#1997=VECTOR('',#7188,1000.);
#1998=VECTOR('',#7191,1000.);
#1999=VECTOR('',#7192,1000.);
#2000=VECTOR('',#7195,1000.);
#2001=VECTOR('',#7196,1000.);
#2002=VECTOR('',#7199,1000.);
#2003=VECTOR('',#7200,1000.);
#2004=VECTOR('',#7203,1000.);
#2005=VECTOR('',#7204,1000.);
#2006=VECTOR('',#7207,1000.);
#2007=VECTOR('',#7208,1000.);
#2008=VECTOR('',#7211,1000.);
#2009=VECTOR('',#7212,1000.);
#2010=VECTOR('',#7215,1000.);
#2011=VECTOR('',#7216,1000.);
#2012=VECTOR('',#7219,1000.);
#2013=VECTOR('',#7220,1000.);
#2014=VECTOR('',#7223,1000.);
#2015=VECTOR('',#7224,1000.);
#2016=VECTOR('',#7227,1000.);
#2017=VECTOR('',#7228,1000.);
#2018=VECTOR('',#7231,1000.);
#2019=VECTOR('',#7232,1000.);
#2020=VECTOR('',#7235,1000.);
#2021=VECTOR('',#7236,1000.);
#2022=VECTOR('',#7239,1000.);
#2023=VECTOR('',#7240,1000.);
#2024=VECTOR('',#7243,1000.);
#2025=VECTOR('',#7244,1000.);
#2026=VECTOR('',#7257,2.5);
#2027=VECTOR('',#7264,2.5);
#2028=VECTOR('',#7271,1000.);
#2029=VECTOR('',#7274,1000.);
#2030=VECTOR('',#7279,1000.);
#2031=VECTOR('',#7282,1000.);
#2032=VECTOR('',#7285,1000.);
#2033=VECTOR('',#7286,1000.);
#2034=VECTOR('',#7289,1000.);
#2035=VECTOR('',#7292,1000.);
#2036=VECTOR('',#7299,1732.05080756886);
#2037=VECTOR('',#7324,1.61);
#2038=VECTOR('',#7329,2.);
#2039=VECTOR('',#7334,3.8);
#2040=VECTOR('',#7343,1000.);
#2041=VECTOR('',#7344,1000.);
#2042=VECTOR('',#7345,1000.);
#2043=VECTOR('',#7346,1000.);
#2044=VECTOR('',#7347,1000.);
#2045=VECTOR('',#7348,1000.);
#2046=VECTOR('',#7355,1000.);
#2047=VECTOR('',#7356,1000.);
#2048=VECTOR('',#7357,1000.);
#2049=VECTOR('',#7358,1000.);
#2050=VECTOR('',#7361,1000.);
#2051=VECTOR('',#7362,1000.);
#2052=VECTOR('',#7363,1000.);
#2053=VECTOR('',#7366,1000.);
#2054=VECTOR('',#7367,1000.);
#2055=VECTOR('',#7368,1000.);
#2056=VECTOR('',#7371,1000.);
#2057=VECTOR('',#7372,1000.);
#2058=VECTOR('',#7373,1000.);
#2059=VECTOR('',#7376,1000.);
#2060=VECTOR('',#7377,1000.);
#2061=VECTOR('',#7378,1000.);
#2062=VECTOR('',#7381,1000.);
#2063=VECTOR('',#7382,1000.);
#2064=VECTOR('',#7399,1732.05080756886);
#2065=VECTOR('',#7424,1.61);
#2066=VECTOR('',#7429,2.);
#2067=VECTOR('',#7434,3.8);
#2068=VECTOR('',#7443,1000.);
#2069=VECTOR('',#7444,1000.);
#2070=VECTOR('',#7445,1000.);
#2071=VECTOR('',#7446,1000.);
#2072=VECTOR('',#7447,1000.);
#2073=VECTOR('',#7448,1000.);
#2074=VECTOR('',#7455,1000.);
#2075=VECTOR('',#7456,1000.);
#2076=VECTOR('',#7457,1000.);
#2077=VECTOR('',#7458,1000.);
#2078=VECTOR('',#7461,1000.);
#2079=VECTOR('',#7462,1000.);
#2080=VECTOR('',#7463,1000.);
#2081=VECTOR('',#7466,1000.);
#2082=VECTOR('',#7467,1000.);
#2083=VECTOR('',#7468,1000.);
#2084=VECTOR('',#7471,1000.);
#2085=VECTOR('',#7472,1000.);
#2086=VECTOR('',#7473,1000.);
#2087=VECTOR('',#7476,1000.);
#2088=VECTOR('',#7477,1000.);
#2089=VECTOR('',#7478,1000.);
#2090=VECTOR('',#7481,1000.);
#2091=VECTOR('',#7482,1000.);
#2092=VECTOR('',#7499,1732.05080756886);
#2093=VECTOR('',#7524,1.61);
#2094=VECTOR('',#7529,2.);
#2095=VECTOR('',#7534,3.8);
#2096=VECTOR('',#7543,1000.);
#2097=VECTOR('',#7544,1000.);
#2098=VECTOR('',#7545,1000.);
#2099=VECTOR('',#7546,1000.);
#2100=VECTOR('',#7547,1000.);
#2101=VECTOR('',#7548,1000.);
#2102=VECTOR('',#7555,1000.);
#2103=VECTOR('',#7556,1000.);
#2104=VECTOR('',#7557,1000.);
#2105=VECTOR('',#7558,1000.);
#2106=VECTOR('',#7561,1000.);
#2107=VECTOR('',#7562,1000.);
#2108=VECTOR('',#7563,1000.);
#2109=VECTOR('',#7566,1000.);
#2110=VECTOR('',#7567,1000.);
#2111=VECTOR('',#7568,1000.);
#2112=VECTOR('',#7571,1000.);
#2113=VECTOR('',#7572,1000.);
#2114=VECTOR('',#7573,1000.);
#2115=VECTOR('',#7576,1000.);
#2116=VECTOR('',#7577,1000.);
#2117=VECTOR('',#7578,1000.);
#2118=VECTOR('',#7581,1000.);
#2119=VECTOR('',#7582,1000.);
#2120=VECTOR('',#7599,1732.05080756886);
#2121=VECTOR('',#7624,1.2195);
#2122=VECTOR('',#7629,1.5);
#2123=VECTOR('',#7634,2.85);
#2124=VECTOR('',#7643,1000.);
#2125=VECTOR('',#7644,1000.);
#2126=VECTOR('',#7645,1000.);
#2127=VECTOR('',#7646,1000.);
#2128=VECTOR('',#7647,1000.);
#2129=VECTOR('',#7648,1000.);
#2130=VECTOR('',#7655,1000.);
#2131=VECTOR('',#7656,1000.);
#2132=VECTOR('',#7657,1000.);
#2133=VECTOR('',#7658,1000.);
#2134=VECTOR('',#7661,1000.);
#2135=VECTOR('',#7662,1000.);
#2136=VECTOR('',#7663,1000.);
#2137=VECTOR('',#7666,1000.);
#2138=VECTOR('',#7667,1000.);
#2139=VECTOR('',#7668,1000.);
#2140=VECTOR('',#7671,1000.);
#2141=VECTOR('',#7672,1000.);
#2142=VECTOR('',#7673,1000.);
#2143=VECTOR('',#7676,1000.);
#2144=VECTOR('',#7677,1000.);
#2145=VECTOR('',#7678,1000.);
#2146=VECTOR('',#7681,1000.);
#2147=VECTOR('',#7682,1000.);
#2148=CIRCLE('',#5682,1.99999999999998);
#2149=CIRCLE('',#5683,1.99999999999997);
#2150=CIRCLE('',#5685,1.99999999999998);
#2151=CIRCLE('',#5686,1.99999999999997);
#2152=CIRCLE('',#5688,2.);
#2153=CIRCLE('',#5689,2.);
#2154=CIRCLE('',#5691,2.5);
#2155=CIRCLE('',#5692,2.5);
#2156=CIRCLE('',#5694,2.5);
#2157=CIRCLE('',#5695,2.5);
#2158=CIRCLE('',#5697,2.5);
#2159=CIRCLE('',#5698,2.5);
#2160=CIRCLE('',#5700,2.5);
#2161=CIRCLE('',#5701,2.5);
#2162=CIRCLE('',#5703,8.);
#2163=CIRCLE('',#5704,8.00000000000001);
#2164=CIRCLE('',#5707,8.);
#2165=CIRCLE('',#5708,8.);
#2166=CIRCLE('',#5711,8.);
#2167=CIRCLE('',#5712,8.);
#2168=CIRCLE('',#5715,8.00000000000001);
#2169=CIRCLE('',#5716,8.00000000000001);
#2170=CIRCLE('',#5721,1.99999999999998);
#2171=CIRCLE('',#5722,1.99999999999998);
#2172=CIRCLE('',#5724,1.99999999999998);
#2173=CIRCLE('',#5725,1.99999999999998);
#2174=CIRCLE('',#5727,2.5);
#2175=CIRCLE('',#5728,2.5);
#2176=CIRCLE('',#5730,2.5);
#2177=CIRCLE('',#5731,2.5);
#2178=CIRCLE('',#5733,8.00000000000001);
#2179=CIRCLE('',#5734,8.);
#2180=CIRCLE('',#5736,2.5);
#2181=CIRCLE('',#5737,2.5);
#2182=CIRCLE('',#5739,2.5);
#2183=CIRCLE('',#5740,2.5);
#2184=CIRCLE('',#5742,2.);
#2185=CIRCLE('',#5743,2.);
#2186=CIRCLE('',#5746,8.);
#2187=CIRCLE('',#5747,8.00000000000001);
#2188=CIRCLE('',#5750,8.);
#2189=CIRCLE('',#5751,8.);
#2190=CIRCLE('',#5754,8.);
#2191=CIRCLE('',#5755,8.);
#2192=CIRCLE('',#5785,3.5);
#2193=CIRCLE('',#5786,3.5);
#2194=CIRCLE('',#5788,4.5);
#2195=CIRCLE('',#5789,4.5);
#2196=CIRCLE('',#5791,3.5);
#2197=CIRCLE('',#5792,3.5);
#2198=CIRCLE('',#5794,2.5);
#2199=CIRCLE('',#5795,2.5);
#2200=CIRCLE('',#5797,2.5);
#2201=CIRCLE('',#5798,2.5);
#2202=CIRCLE('',#5802,6.50000000000001);
#2203=CIRCLE('',#5803,10.);
#2204=CIRCLE('',#5804,22.9999999999999);
#2205=CIRCLE('',#5805,4.5);
#2206=CIRCLE('',#5806,12.);
#2207=CIRCLE('',#5807,24.9999999999999);
#2208=CIRCLE('',#5808,24.9999999999999);
#2209=CIRCLE('',#5810,22.9999999999999);
#2210=CIRCLE('',#5811,10.);
#2211=CIRCLE('',#5812,6.50000000000001);
#2212=CIRCLE('',#5813,24.9999999999999);
#2213=CIRCLE('',#5814,24.9999999999999);
#2214=CIRCLE('',#5815,12.);
#2215=CIRCLE('',#5841,24.9999999999999);
#2216=CIRCLE('',#5847,24.9999999999999);
#2217=CIRCLE('',#5851,4.5);
#2218=CIRCLE('',#5857,12.);
#2219=CIRCLE('',#5864,12.);
#2220=CIRCLE('',#5873,24.9999999999999);
#2221=CIRCLE('',#5881,24.9999999999999);
#2222=CIRCLE('',#5886,7.);
#2223=CIRCLE('',#5887,7.);
#2224=CIRCLE('',#5889,14.);
#2225=CIRCLE('',#5890,14.);
#2226=CIRCLE('',#5892,7.);
#2227=CIRCLE('',#5893,7.);
#2228=CIRCLE('',#5895,14.);
#2229=CIRCLE('',#5896,14.);
#2230=CIRCLE('',#5898,2.5);
#2231=CIRCLE('',#5899,2.5);
#2232=CIRCLE('',#5901,16.25);
#2233=CIRCLE('',#5902,16.25);
#2234=CIRCLE('',#5906,19.);
#2235=CIRCLE('',#5907,16.25);
#2236=CIRCLE('',#5908,19.);
#2237=CIRCLE('',#5909,16.25);
#2238=CIRCLE('',#5910,19.);
#2239=CIRCLE('',#5911,16.25);
#2240=CIRCLE('',#5912,19.);
#2241=CIRCLE('',#5913,16.25);
#2242=CIRCLE('',#5914,19.);
#2243=CIRCLE('',#5915,16.25);
#2244=CIRCLE('',#5916,19.);
#2245=CIRCLE('',#5917,16.25);
#2246=CIRCLE('',#5918,19.);
#2247=CIRCLE('',#5919,16.25);
#2248=CIRCLE('',#5920,19.);
#2249=CIRCLE('',#5921,16.25);
#2250=CIRCLE('',#5922,19.);
#2251=CIRCLE('',#5923,19.);
#2252=CIRCLE('',#5924,16.25);
#2253=CIRCLE('',#5925,19.);
#2254=CIRCLE('',#5926,16.25);
#2255=CIRCLE('',#5927,19.);
#2256=CIRCLE('',#5928,16.25);
#2257=CIRCLE('',#5929,19.);
#2258=CIRCLE('',#5930,16.25);
#2259=CIRCLE('',#5931,19.);
#2260=CIRCLE('',#5932,16.25);
#2261=CIRCLE('',#5933,19.);
#2262=CIRCLE('',#5934,16.25);
#2263=CIRCLE('',#5935,19.);
#2264=CIRCLE('',#5936,16.25);
#2265=CIRCLE('',#5937,19.);
#2266=CIRCLE('',#5938,16.25);
#2267=CIRCLE('',#5939,19.);
#2268=CIRCLE('',#5940,16.25);
#2269=CIRCLE('',#5941,19.);
#2270=CIRCLE('',#5942,16.25);
#2271=CIRCLE('',#5943,19.);
#2272=CIRCLE('',#5944,16.25);
#2273=CIRCLE('',#5946,16.25);
#2274=CIRCLE('',#5947,19.);
#2275=CIRCLE('',#5948,16.25);
#2276=CIRCLE('',#5949,19.);
#2277=CIRCLE('',#5950,16.25);
#2278=CIRCLE('',#5951,19.);
#2279=CIRCLE('',#5952,16.25);
#2280=CIRCLE('',#5953,19.);
#2281=CIRCLE('',#5954,16.25);
#2282=CIRCLE('',#5955,19.);
#2283=CIRCLE('',#5956,16.25);
#2284=CIRCLE('',#5957,19.);
#2285=CIRCLE('',#5958,16.25);
#2286=CIRCLE('',#5959,19.);
#2287=CIRCLE('',#5960,16.25);
#2288=CIRCLE('',#5961,19.);
#2289=CIRCLE('',#5962,16.25);
#2290=CIRCLE('',#5963,19.);
#2291=CIRCLE('',#5964,16.25);
#2292=CIRCLE('',#5965,19.);
#2293=CIRCLE('',#5966,16.25);
#2294=CIRCLE('',#5967,19.);
#2295=CIRCLE('',#5968,19.);
#2296=CIRCLE('',#5969,16.25);
#2297=CIRCLE('',#5970,19.);
#2298=CIRCLE('',#5971,16.25);
#2299=CIRCLE('',#5972,19.);
#2300=CIRCLE('',#5973,16.25);
#2301=CIRCLE('',#5974,19.);
#2302=CIRCLE('',#5975,16.25);
#2303=CIRCLE('',#5976,19.);
#2304=CIRCLE('',#5977,16.25);
#2305=CIRCLE('',#5978,19.);
#2306=CIRCLE('',#5979,16.25);
#2307=CIRCLE('',#5980,19.);
#2308=CIRCLE('',#5981,16.25);
#2309=CIRCLE('',#5982,19.);
#2310=CIRCLE('',#5983,16.25);
#2311=CIRCLE('',#5984,19.);
#2312=CIRCLE('',#6028,2.5);
#2313=CIRCLE('',#6029,2.5);
#2314=CIRCLE('',#6031,2.5);
#2315=CIRCLE('',#6032,2.5);
#2316=CIRCLE('',#6034,5.);
#2317=CIRCLE('',#6035,5.);
#2318=CIRCLE('',#6037,5.);
#2319=CIRCLE('',#6038,5.);
#2320=CIRCLE('',#6045,1.25);
#2321=CIRCLE('',#6046,1.25);
#2322=CIRCLE('',#6047,1.25);
#2323=CIRCLE('',#6048,1.25);
#2324=CIRCLE('',#6049,1.25);
#2325=CIRCLE('',#6050,1.25);
#2326=CIRCLE('',#6052,2.2);
#2327=CIRCLE('',#6053,0.2);
#2328=CIRCLE('',#6054,2.);
#2329=CIRCLE('',#6056,2.);
#2330=CIRCLE('',#6057,1.61);
#2331=CIRCLE('',#6060,3.8);
#2332=CIRCLE('',#6061,3.8);
#2333=CIRCLE('',#6063,1.9);
#2334=CIRCLE('',#6081,1.25);
#2335=CIRCLE('',#6082,1.25);
#2336=CIRCLE('',#6083,1.25);
#2337=CIRCLE('',#6084,1.25);
#2338=CIRCLE('',#6085,1.25);
#2339=CIRCLE('',#6086,1.25);
#2340=CIRCLE('',#6088,2.2);
#2341=CIRCLE('',#6089,0.2);
#2342=CIRCLE('',#6090,2.);
#2343=CIRCLE('',#6092,2.);
#2344=CIRCLE('',#6093,1.61);
#2345=CIRCLE('',#6096,3.8);
#2346=CIRCLE('',#6097,3.8);
#2347=CIRCLE('',#6099,1.9);
#2348=CIRCLE('',#6117,1.25);
#2349=CIRCLE('',#6118,1.25);
#2350=CIRCLE('',#6119,1.25);
#2351=CIRCLE('',#6120,1.25);
#2352=CIRCLE('',#6121,1.25);
#2353=CIRCLE('',#6122,1.25);
#2354=CIRCLE('',#6124,2.2);
#2355=CIRCLE('',#6125,0.2);
#2356=CIRCLE('',#6126,2.);
#2357=CIRCLE('',#6128,2.);
#2358=CIRCLE('',#6129,1.61);
#2359=CIRCLE('',#6132,3.8);
#2360=CIRCLE('',#6133,3.8);
#2361=CIRCLE('',#6135,1.9);
#2362=CIRCLE('',#6153,1.);
#2363=CIRCLE('',#6154,1.);
#2364=CIRCLE('',#6155,1.);
#2365=CIRCLE('',#6156,1.);
#2366=CIRCLE('',#6157,1.);
#2367=CIRCLE('',#6158,1.);
#2368=CIRCLE('',#6160,1.6);
#2369=CIRCLE('',#6161,0.1);
#2370=CIRCLE('',#6162,1.5);
#2371=CIRCLE('',#6164,1.5);
#2372=CIRCLE('',#6165,1.2195);
#2373=CIRCLE('',#6168,2.85);
#2374=CIRCLE('',#6169,2.85);
#2375=CIRCLE('',#6171,1.425);
#2376=VERTEX_POINT('',#7768);
#2377=VERTEX_POINT('',#7770);
#2378=VERTEX_POINT('',#7774);
#2379=VERTEX_POINT('',#7776);
#2380=VERTEX_POINT('',#7780);
#2381=VERTEX_POINT('',#7782);
#2382=VERTEX_POINT('',#7786);
#2383=VERTEX_POINT('',#7788);
#2384=VERTEX_POINT('',#7792);
#2385=VERTEX_POINT('',#7794);
#2386=VERTEX_POINT('',#7798);
#2387=VERTEX_POINT('',#7800);
#2388=VERTEX_POINT('',#7804);
#2389=VERTEX_POINT('',#7806);
#2390=VERTEX_POINT('',#7810);
#2391=VERTEX_POINT('',#7811);
#2392=VERTEX_POINT('',#7813);
#2393=VERTEX_POINT('',#7815);
#2394=VERTEX_POINT('',#7819);
#2395=VERTEX_POINT('',#7821);
#2396=VERTEX_POINT('',#7825);
#2397=VERTEX_POINT('',#7827);
#2398=VERTEX_POINT('',#7831);
#2399=VERTEX_POINT('',#7833);
#2400=VERTEX_POINT('',#7837);
#2401=VERTEX_POINT('',#7839);
#2402=VERTEX_POINT('',#7843);
#2403=VERTEX_POINT('',#7845);
#2404=VERTEX_POINT('',#7849);
#2405=VERTEX_POINT('',#7851);
#2406=VERTEX_POINT('',#7860);
#2407=VERTEX_POINT('',#7862);
#2408=VERTEX_POINT('',#7866);
#2409=VERTEX_POINT('',#7868);
#2410=VERTEX_POINT('',#7872);
#2411=VERTEX_POINT('',#7874);
#2412=VERTEX_POINT('',#7878);
#2413=VERTEX_POINT('',#7880);
#2414=VERTEX_POINT('',#7884);
#2415=VERTEX_POINT('',#7885);
#2416=VERTEX_POINT('',#7887);
#2417=VERTEX_POINT('',#7889);
#2418=VERTEX_POINT('',#7893);
#2419=VERTEX_POINT('',#7895);
#2420=VERTEX_POINT('',#7899);
#2421=VERTEX_POINT('',#7901);
#2422=VERTEX_POINT('',#7905);
#2423=VERTEX_POINT('',#7907);
#2424=VERTEX_POINT('',#7911);
#2425=VERTEX_POINT('',#7913);
#2426=VERTEX_POINT('',#7917);
#2427=VERTEX_POINT('',#7919);
#2428=VERTEX_POINT('',#7923);
#2429=VERTEX_POINT('',#7925);
#2430=VERTEX_POINT('',#7929);
#2431=VERTEX_POINT('',#7931);
#2432=VERTEX_POINT('',#7935);
#2433=VERTEX_POINT('',#7937);
#2434=VERTEX_POINT('',#7941);
#2435=VERTEX_POINT('',#7943);
#2436=VERTEX_POINT('',#7952);
#2437=VERTEX_POINT('',#7953);
#2438=VERTEX_POINT('',#7955);
#2439=VERTEX_POINT('',#7957);
#2440=VERTEX_POINT('',#7961);
#2441=VERTEX_POINT('',#7963);
#2442=VERTEX_POINT('',#7967);
#2443=VERTEX_POINT('',#7969);
#2444=VERTEX_POINT('',#7973);
#2445=VERTEX_POINT('',#7975);
#2446=VERTEX_POINT('',#7979);
#2447=VERTEX_POINT('',#7981);
#2448=VERTEX_POINT('',#7990);
#2449=VERTEX_POINT('',#7991);
#2450=VERTEX_POINT('',#7993);
#2451=VERTEX_POINT('',#7995);
#2452=VERTEX_POINT('',#7999);
#2453=VERTEX_POINT('',#8001);
#2454=VERTEX_POINT('',#8005);
#2455=VERTEX_POINT('',#8007);
#2456=VERTEX_POINT('',#8011);
#2457=VERTEX_POINT('',#8013);
#2458=VERTEX_POINT('',#8017);
#2459=VERTEX_POINT('',#8019);
#2460=VERTEX_POINT('',#8028);
#2461=VERTEX_POINT('',#8029);
#2462=VERTEX_POINT('',#8031);
#2463=VERTEX_POINT('',#8033);
#2464=VERTEX_POINT('',#8037);
#2465=VERTEX_POINT('',#8039);
#2466=VERTEX_POINT('',#8043);
#2467=VERTEX_POINT('',#8045);
#2468=VERTEX_POINT('',#8049);
#2469=VERTEX_POINT('',#8051);
#2470=VERTEX_POINT('',#8055);
#2471=VERTEX_POINT('',#8057);
#2472=VERTEX_POINT('',#8067);
#2473=VERTEX_POINT('',#8069);
#2474=VERTEX_POINT('',#8073);
#2475=VERTEX_POINT('',#8074);
#2476=VERTEX_POINT('',#8076);
#2477=VERTEX_POINT('',#8078);
#2478=VERTEX_POINT('',#8082);
#2479=VERTEX_POINT('',#8084);
#2480=VERTEX_POINT('',#8088);
#2481=VERTEX_POINT('',#8090);
#2482=VERTEX_POINT('',#8094);
#2483=VERTEX_POINT('',#8096);
#2484=VERTEX_POINT('',#8102);
#2485=VERTEX_POINT('',#8103);
#2486=VERTEX_POINT('',#8105);
#2487=VERTEX_POINT('',#8107);
#2488=VERTEX_POINT('',#8109);
#2489=VERTEX_POINT('',#8111);
#2490=VERTEX_POINT('',#8113);
#2491=VERTEX_POINT('',#8115);
#2492=VERTEX_POINT('',#8117);
#2493=VERTEX_POINT('',#8119);
#2494=VERTEX_POINT('',#8121);
#2495=VERTEX_POINT('',#8123);
#2496=VERTEX_POINT('',#8125);
#2497=VERTEX_POINT('',#8127);
#2498=VERTEX_POINT('',#8129);
#2499=VERTEX_POINT('',#8131);
#2500=VERTEX_POINT('',#8133);
#2501=VERTEX_POINT('',#8135);
#2502=VERTEX_POINT('',#8137);
#2503=VERTEX_POINT('',#8139);
#2504=VERTEX_POINT('',#8142);
#2505=VERTEX_POINT('',#8143);
#2506=VERTEX_POINT('',#8145);
#2507=VERTEX_POINT('',#8147);
#2508=VERTEX_POINT('',#8149);
#2509=VERTEX_POINT('',#8151);
#2510=VERTEX_POINT('',#8153);
#2511=VERTEX_POINT('',#8155);
#2512=VERTEX_POINT('',#8158);
#2513=VERTEX_POINT('',#8159);
#2514=VERTEX_POINT('',#8161);
#2515=VERTEX_POINT('',#8163);
#2516=VERTEX_POINT('',#8165);
#2517=VERTEX_POINT('',#8168);
#2518=VERTEX_POINT('',#8169);
#2519=VERTEX_POINT('',#8171);
#2520=VERTEX_POINT('',#8173);
#2521=VERTEX_POINT('',#8175);
#2522=VERTEX_POINT('',#8179);
#2523=VERTEX_POINT('',#8180);
#2524=VERTEX_POINT('',#8182);
#2525=VERTEX_POINT('',#8184);
#2526=VERTEX_POINT('',#8186);
#2527=VERTEX_POINT('',#8188);
#2528=VERTEX_POINT('',#8190);
#2529=VERTEX_POINT('',#8192);
#2530=VERTEX_POINT('',#8194);
#2531=VERTEX_POINT('',#8196);
#2532=VERTEX_POINT('',#8198);
#2533=VERTEX_POINT('',#8200);
#2534=VERTEX_POINT('',#8202);
#2535=VERTEX_POINT('',#8204);
#2536=VERTEX_POINT('',#8206);
#2537=VERTEX_POINT('',#8208);
#2538=VERTEX_POINT('',#8210);
#2539=VERTEX_POINT('',#8212);
#2540=VERTEX_POINT('',#8214);
#2541=VERTEX_POINT('',#8216);
#2542=VERTEX_POINT('',#8219);
#2543=VERTEX_POINT('',#8220);
#2544=VERTEX_POINT('',#8222);
#2545=VERTEX_POINT('',#8224);
#2546=VERTEX_POINT('',#8226);
#2547=VERTEX_POINT('',#8229);
#2548=VERTEX_POINT('',#8230);
#2549=VERTEX_POINT('',#8232);
#2550=VERTEX_POINT('',#8234);
#2551=VERTEX_POINT('',#8236);
#2552=VERTEX_POINT('',#8239);
#2553=VERTEX_POINT('',#8241);
#2554=VERTEX_POINT('',#8243);
#2555=VERTEX_POINT('',#8245);
#2556=VERTEX_POINT('',#8247);
#2557=VERTEX_POINT('',#8249);
#2558=VERTEX_POINT('',#8293);
#2559=VERTEX_POINT('',#8295);
#2560=VERTEX_POINT('',#8299);
#2561=VERTEX_POINT('',#8303);
#2562=VERTEX_POINT('',#8307);
#2563=VERTEX_POINT('',#8314);
#2564=VERTEX_POINT('',#8316);
#2565=VERTEX_POINT('',#8320);
#2566=VERTEX_POINT('',#8324);
#2567=VERTEX_POINT('',#8328);
#2568=VERTEX_POINT('',#8335);
#2569=VERTEX_POINT('',#8337);
#2570=VERTEX_POINT('',#8341);
#2571=VERTEX_POINT('',#8345);
#2572=VERTEX_POINT('',#8349);
#2573=VERTEX_POINT('',#8353);
#2574=VERTEX_POINT('',#8357);
#2575=VERTEX_POINT('',#8361);
#2576=VERTEX_POINT('',#8368);
#2577=VERTEX_POINT('',#8372);
#2578=VERTEX_POINT('',#8376);
#2579=VERTEX_POINT('',#8380);
#2580=VERTEX_POINT('',#8384);
#2581=VERTEX_POINT('',#8388);
#2582=VERTEX_POINT('',#8395);
#2583=VERTEX_POINT('',#8397);
#2584=VERTEX_POINT('',#8401);
#2585=VERTEX_POINT('',#8405);
#2586=VERTEX_POINT('',#8409);
#2587=VERTEX_POINT('',#8416);
#2588=VERTEX_POINT('',#8418);
#2589=VERTEX_POINT('',#8422);
#2590=VERTEX_POINT('',#8426);
#2591=VERTEX_POINT('',#8430);
#2592=VERTEX_POINT('',#8438);
#2593=VERTEX_POINT('',#8440);
#2594=VERTEX_POINT('',#8444);
#2595=VERTEX_POINT('',#8446);
#2596=VERTEX_POINT('',#8450);
#2597=VERTEX_POINT('',#8452);
#2598=VERTEX_POINT('',#8456);
#2599=VERTEX_POINT('',#8458);
#2600=VERTEX_POINT('',#8462);
#2601=VERTEX_POINT('',#8464);
#2602=VERTEX_POINT('',#8468);
#2603=VERTEX_POINT('',#8469);
#2604=VERTEX_POINT('',#8471);
#2605=VERTEX_POINT('',#8473);
#2606=VERTEX_POINT('',#8479);
#2607=VERTEX_POINT('',#8480);
#2608=VERTEX_POINT('',#8504);
#2609=VERTEX_POINT('',#8506);
#2610=VERTEX_POINT('',#8530);
#2611=VERTEX_POINT('',#8532);
#2612=VERTEX_POINT('',#8556);
#2613=VERTEX_POINT('',#8558);
#2614=VERTEX_POINT('',#8582);
#2615=VERTEX_POINT('',#8584);
#2616=VERTEX_POINT('',#8608);
#2617=VERTEX_POINT('',#8610);
#2618=VERTEX_POINT('',#8634);
#2619=VERTEX_POINT('',#8636);
#2620=VERTEX_POINT('',#8660);
#2621=VERTEX_POINT('',#8662);
#2622=VERTEX_POINT('',#8686);
#2623=VERTEX_POINT('',#8688);
#2624=VERTEX_POINT('',#8712);
#2625=VERTEX_POINT('',#8714);
#2626=VERTEX_POINT('',#8738);
#2627=VERTEX_POINT('',#8740);
#2628=VERTEX_POINT('',#8764);
#2629=VERTEX_POINT('',#8766);
#2630=VERTEX_POINT('',#8790);
#2631=VERTEX_POINT('',#8792);
#2632=VERTEX_POINT('',#8816);
#2633=VERTEX_POINT('',#8818);
#2634=VERTEX_POINT('',#8842);
#2635=VERTEX_POINT('',#8844);
#2636=VERTEX_POINT('',#8868);
#2637=VERTEX_POINT('',#8870);
#2638=VERTEX_POINT('',#8894);
#2639=VERTEX_POINT('',#8896);
#2640=VERTEX_POINT('',#8920);
#2641=VERTEX_POINT('',#8945);
#2642=VERTEX_POINT('',#8969);
#2643=VERTEX_POINT('',#8971);
#2644=VERTEX_POINT('',#8995);
#2645=VERTEX_POINT('',#8997);
#2646=VERTEX_POINT('',#9021);
#2647=VERTEX_POINT('',#9023);
#2648=VERTEX_POINT('',#9047);
#2649=VERTEX_POINT('',#9049);
#2650=VERTEX_POINT('',#9073);
#2651=VERTEX_POINT('',#9075);
#2652=VERTEX_POINT('',#9099);
#2653=VERTEX_POINT('',#9101);
#2654=VERTEX_POINT('',#9125);
#2655=VERTEX_POINT('',#9127);
#2656=VERTEX_POINT('',#9151);
#2657=VERTEX_POINT('',#9153);
#2658=VERTEX_POINT('',#9177);
#2659=VERTEX_POINT('',#9179);
#2660=VERTEX_POINT('',#9203);
#2661=VERTEX_POINT('',#9205);
#2662=VERTEX_POINT('',#9229);
#2663=VERTEX_POINT('',#9231);
#2664=VERTEX_POINT('',#9255);
#2665=VERTEX_POINT('',#9257);
#2666=VERTEX_POINT('',#9281);
#2667=VERTEX_POINT('',#9283);
#2668=VERTEX_POINT('',#9307);
#2669=VERTEX_POINT('',#9309);
#2670=VERTEX_POINT('',#9333);
#2671=VERTEX_POINT('',#9335);
#2672=VERTEX_POINT('',#9359);
#2673=VERTEX_POINT('',#9361);
#2674=VERTEX_POINT('',#9385);
#2675=VERTEX_POINT('',#9387);
#2676=VERTEX_POINT('',#9411);
#2677=VERTEX_POINT('',#9413);
#2678=VERTEX_POINT('',#9437);
#2679=VERTEX_POINT('',#9439);
#2680=VERTEX_POINT('',#9463);
#2681=VERTEX_POINT('',#9465);
#2682=VERTEX_POINT('',#9489);
#2683=VERTEX_POINT('',#9491);
#2684=VERTEX_POINT('',#9517);
#2685=VERTEX_POINT('',#9518);
#2686=VERTEX_POINT('',#9542);
#2687=VERTEX_POINT('',#9544);
#2688=VERTEX_POINT('',#9568);
#2689=VERTEX_POINT('',#9570);
#2690=VERTEX_POINT('',#9594);
#2691=VERTEX_POINT('',#9596);
#2692=VERTEX_POINT('',#9620);
#2693=VERTEX_POINT('',#9622);
#2694=VERTEX_POINT('',#9646);
#2695=VERTEX_POINT('',#9648);
#2696=VERTEX_POINT('',#9672);
#2697=VERTEX_POINT('',#9674);
#2698=VERTEX_POINT('',#9698);
#2699=VERTEX_POINT('',#9700);
#2700=VERTEX_POINT('',#9724);
#2701=VERTEX_POINT('',#9726);
#2702=VERTEX_POINT('',#9750);
#2703=VERTEX_POINT('',#9752);
#2704=VERTEX_POINT('',#9776);
#2705=VERTEX_POINT('',#9778);
#2706=VERTEX_POINT('',#9802);
#2707=VERTEX_POINT('',#9804);
#2708=VERTEX_POINT('',#9828);
#2709=VERTEX_POINT('',#9830);
#2710=VERTEX_POINT('',#9854);
#2711=VERTEX_POINT('',#9856);
#2712=VERTEX_POINT('',#9880);
#2713=VERTEX_POINT('',#9882);
#2714=VERTEX_POINT('',#9906);
#2715=VERTEX_POINT('',#9908);
#2716=VERTEX_POINT('',#9932);
#2717=VERTEX_POINT('',#9934);
#2718=VERTEX_POINT('',#9958);
#2719=VERTEX_POINT('',#9960);
#2720=VERTEX_POINT('',#9984);
#2721=VERTEX_POINT('',#9986);
#2722=VERTEX_POINT('',#10010);
#2723=VERTEX_POINT('',#10012);
#2724=VERTEX_POINT('',#10036);
#2725=VERTEX_POINT('',#10038);
#2726=VERTEX_POINT('',#10062);
#2727=VERTEX_POINT('',#10064);
#2728=VERTEX_POINT('',#10088);
#2729=VERTEX_POINT('',#10113);
#2730=VERTEX_POINT('',#10137);
#2731=VERTEX_POINT('',#10139);
#2732=VERTEX_POINT('',#10163);
#2733=VERTEX_POINT('',#10165);
#2734=VERTEX_POINT('',#10189);
#2735=VERTEX_POINT('',#10191);
#2736=VERTEX_POINT('',#10215);
#2737=VERTEX_POINT('',#10217);
#2738=VERTEX_POINT('',#10241);
#2739=VERTEX_POINT('',#10243);
#2740=VERTEX_POINT('',#10267);
#2741=VERTEX_POINT('',#10269);
#2742=VERTEX_POINT('',#10293);
#2743=VERTEX_POINT('',#10295);
#2744=VERTEX_POINT('',#10319);
#2745=VERTEX_POINT('',#10321);
#2746=VERTEX_POINT('',#10345);
#2747=VERTEX_POINT('',#10347);
#2748=VERTEX_POINT('',#10371);
#2749=VERTEX_POINT('',#10373);
#2750=VERTEX_POINT('',#10397);
#2751=VERTEX_POINT('',#10399);
#2752=VERTEX_POINT('',#10423);
#2753=VERTEX_POINT('',#10425);
#2754=VERTEX_POINT('',#10449);
#2755=VERTEX_POINT('',#10451);
#2756=VERTEX_POINT('',#10475);
#2757=VERTEX_POINT('',#10477);
#2758=VERTEX_POINT('',#10501);
#2759=VERTEX_POINT('',#10503);
#2760=VERTEX_POINT('',#10527);
#2761=VERTEX_POINT('',#10529);
#2762=VERTEX_POINT('',#12515);
#2763=VERTEX_POINT('',#12517);
#2764=VERTEX_POINT('',#12521);
#2765=VERTEX_POINT('',#12523);
#2766=VERTEX_POINT('',#12527);
#2767=VERTEX_POINT('',#12528);
#2768=VERTEX_POINT('',#12530);
#2769=VERTEX_POINT('',#12532);
#2770=VERTEX_POINT('',#12536);
#2771=VERTEX_POINT('',#12537);
#2772=VERTEX_POINT('',#12539);
#2773=VERTEX_POINT('',#12541);
#2774=VERTEX_POINT('',#12554);
#2775=VERTEX_POINT('',#12555);
#2776=VERTEX_POINT('',#12557);
#2777=VERTEX_POINT('',#12559);
#2778=VERTEX_POINT('',#12561);
#2779=VERTEX_POINT('',#12563);
#2780=VERTEX_POINT('',#12565);
#2781=VERTEX_POINT('',#12569);
#2782=VERTEX_POINT('',#12571);
#2783=VERTEX_POINT('',#12575);
#2784=VERTEX_POINT('',#12577);
#2785=VERTEX_POINT('',#12583);
#2786=VERTEX_POINT('',#12585);
#2787=VERTEX_POINT('',#12589);
#2788=VERTEX_POINT('',#12592);
#2789=VERTEX_POINT('',#12593);
#2790=VERTEX_POINT('',#12595);
#2791=VERTEX_POINT('',#12597);
#2792=VERTEX_POINT('',#12599);
#2793=VERTEX_POINT('',#12601);
#2794=VERTEX_POINT('',#12607);
#2795=VERTEX_POINT('',#12609);
#2796=VERTEX_POINT('',#12615);
#2797=VERTEX_POINT('',#12620);
#2798=VERTEX_POINT('',#12625);
#2799=VERTEX_POINT('',#12630);
#2800=VERTEX_POINT('',#12644);
#2801=VERTEX_POINT('',#12645);
#2802=VERTEX_POINT('',#12647);
#2803=VERTEX_POINT('',#12649);
#2804=VERTEX_POINT('',#12651);
#2805=VERTEX_POINT('',#12653);
#2806=VERTEX_POINT('',#12655);
#2807=VERTEX_POINT('',#12659);
#2808=VERTEX_POINT('',#12661);
#2809=VERTEX_POINT('',#12665);
#2810=VERTEX_POINT('',#12667);
#2811=VERTEX_POINT('',#12673);
#2812=VERTEX_POINT('',#12675);
#2813=VERTEX_POINT('',#12679);
#2814=VERTEX_POINT('',#12682);
#2815=VERTEX_POINT('',#12683);
#2816=VERTEX_POINT('',#12685);
#2817=VERTEX_POINT('',#12687);
#2818=VERTEX_POINT('',#12689);
#2819=VERTEX_POINT('',#12691);
#2820=VERTEX_POINT('',#12697);
#2821=VERTEX_POINT('',#12699);
#2822=VERTEX_POINT('',#12705);
#2823=VERTEX_POINT('',#12710);
#2824=VERTEX_POINT('',#12715);
#2825=VERTEX_POINT('',#12720);
#2826=VERTEX_POINT('',#12734);
#2827=VERTEX_POINT('',#12735);
#2828=VERTEX_POINT('',#12737);
#2829=VERTEX_POINT('',#12739);
#2830=VERTEX_POINT('',#12741);
#2831=VERTEX_POINT('',#12743);
#2832=VERTEX_POINT('',#12745);
#2833=VERTEX_POINT('',#12749);
#2834=VERTEX_POINT('',#12751);
#2835=VERTEX_POINT('',#12755);
#2836=VERTEX_POINT('',#12757);
#2837=VERTEX_POINT('',#12763);
#2838=VERTEX_POINT('',#12765);
#2839=VERTEX_POINT('',#12769);
#2840=VERTEX_POINT('',#12772);
#2841=VERTEX_POINT('',#12773);
#2842=VERTEX_POINT('',#12775);
#2843=VERTEX_POINT('',#12777);
#2844=VERTEX_POINT('',#12779);
#2845=VERTEX_POINT('',#12781);
#2846=VERTEX_POINT('',#12787);
#2847=VERTEX_POINT('',#12789);
#2848=VERTEX_POINT('',#12795);
#2849=VERTEX_POINT('',#12800);
#2850=VERTEX_POINT('',#12805);
#2851=VERTEX_POINT('',#12810);
#2852=VERTEX_POINT('',#12824);
#2853=VERTEX_POINT('',#12825);
#2854=VERTEX_POINT('',#12827);
#2855=VERTEX_POINT('',#12829);
#2856=VERTEX_POINT('',#12831);
#2857=VERTEX_POINT('',#12833);
#2858=VERTEX_POINT('',#12835);
#2859=VERTEX_POINT('',#12839);
#2860=VERTEX_POINT('',#12841);
#2861=VERTEX_POINT('',#12845);
#2862=VERTEX_POINT('',#12847);
#2863=VERTEX_POINT('',#12853);
#2864=VERTEX_POINT('',#12855);
#2865=VERTEX_POINT('',#12859);
#2866=VERTEX_POINT('',#12862);
#2867=VERTEX_POINT('',#12863);
#2868=VERTEX_POINT('',#12865);
#2869=VERTEX_POINT('',#12867);
#2870=VERTEX_POINT('',#12869);
#2871=VERTEX_POINT('',#12871);
#2872=VERTEX_POINT('',#12877);
#2873=VERTEX_POINT('',#12879);
#2874=VERTEX_POINT('',#12885);
#2875=VERTEX_POINT('',#12890);
#2876=VERTEX_POINT('',#12895);
#2877=VERTEX_POINT('',#12900);
#2878=EDGE_CURVE('',#2376,#2376,#2148,.T.);
#2879=EDGE_CURVE('',#2376,#2377,#1234,.T.);
#2880=EDGE_CURVE('',#2377,#2377,#2149,.T.);
#2881=EDGE_CURVE('',#2378,#2378,#2150,.T.);
#2882=EDGE_CURVE('',#2378,#2379,#1235,.T.);
#2883=EDGE_CURVE('',#2379,#2379,#2151,.T.);
#2884=EDGE_CURVE('',#2380,#2380,#2152,.T.);
#2885=EDGE_CURVE('',#2380,#2381,#1236,.T.);
#2886=EDGE_CURVE('',#2381,#2381,#2153,.T.);
#2887=EDGE_CURVE('',#2382,#2382,#2154,.T.);
#2888=EDGE_CURVE('',#2382,#2383,#1237,.T.);
#2889=EDGE_CURVE('',#2383,#2383,#2155,.T.);
#2890=EDGE_CURVE('',#2384,#2384,#2156,.T.);
#2891=EDGE_CURVE('',#2384,#2385,#1238,.T.);
#2892=EDGE_CURVE('',#2385,#2385,#2157,.T.);
#2893=EDGE_CURVE('',#2386,#2386,#2158,.T.);
#2894=EDGE_CURVE('',#2386,#2387,#1239,.T.);
#2895=EDGE_CURVE('',#2387,#2387,#2159,.T.);
#2896=EDGE_CURVE('',#2388,#2388,#2160,.T.);
#2897=EDGE_CURVE('',#2388,#2389,#1240,.T.);
#2898=EDGE_CURVE('',#2389,#2389,#2161,.T.);
#2899=EDGE_CURVE('',#2390,#2391,#2162,.T.);
#2900=EDGE_CURVE('',#2390,#2392,#1241,.T.);
#2901=EDGE_CURVE('',#2392,#2393,#2163,.T.);
#2902=EDGE_CURVE('',#2391,#2393,#1242,.T.);
#2903=EDGE_CURVE('',#2393,#2394,#1243,.T.);
#2904=EDGE_CURVE('',#2395,#2394,#1244,.T.);
#2905=EDGE_CURVE('',#2391,#2395,#1245,.T.);
#2906=EDGE_CURVE('',#2394,#2396,#2164,.T.);
#2907=EDGE_CURVE('',#2397,#2396,#1246,.T.);
#2908=EDGE_CURVE('',#2395,#2397,#2165,.T.);
#2909=EDGE_CURVE('',#2396,#2398,#1247,.T.);
#2910=EDGE_CURVE('',#2399,#2398,#1248,.T.);
#2911=EDGE_CURVE('',#2397,#2399,#1249,.T.);
#2912=EDGE_CURVE('',#2398,#2400,#2166,.T.);
#2913=EDGE_CURVE('',#2401,#2400,#1250,.T.);
#2914=EDGE_CURVE('',#2399,#2401,#2167,.T.);
#2915=EDGE_CURVE('',#2400,#2402,#1251,.T.);
#2916=EDGE_CURVE('',#2403,#2402,#1252,.T.);
#2917=EDGE_CURVE('',#2401,#2403,#1253,.T.);
#2918=EDGE_CURVE('',#2402,#2404,#2168,.T.);
#2919=EDGE_CURVE('',#2405,#2404,#1254,.T.);
#2920=EDGE_CURVE('',#2403,#2405,#2169,.T.);
#2921=EDGE_CURVE('',#2392,#2404,#1255,.T.);
#2922=EDGE_CURVE('',#2405,#2390,#1256,.T.);
#2923=EDGE_CURVE('',#2406,#2406,#2170,.T.);
#2924=EDGE_CURVE('',#2406,#2407,#1257,.T.);
#2925=EDGE_CURVE('',#2407,#2407,#2171,.T.);
#2926=EDGE_CURVE('',#2408,#2408,#2172,.T.);
#2927=EDGE_CURVE('',#2408,#2409,#1258,.T.);
#2928=EDGE_CURVE('',#2409,#2409,#2173,.T.);
#2929=EDGE_CURVE('',#2410,#2410,#2174,.T.);
#2930=EDGE_CURVE('',#2410,#2411,#1259,.T.);
#2931=EDGE_CURVE('',#2411,#2411,#2175,.T.);
#2932=EDGE_CURVE('',#2412,#2412,#2176,.T.);
#2933=EDGE_CURVE('',#2412,#2413,#1260,.T.);
#2934=EDGE_CURVE('',#2413,#2413,#2177,.T.);
#2935=EDGE_CURVE('',#2414,#2415,#2178,.T.);
#2936=EDGE_CURVE('',#2415,#2416,#1261,.T.);
#2937=EDGE_CURVE('',#2416,#2417,#2179,.T.);
#2938=EDGE_CURVE('',#2414,#2417,#1262,.T.);
#2939=EDGE_CURVE('',#2418,#2418,#2180,.T.);
#2940=EDGE_CURVE('',#2418,#2419,#1263,.T.);
#2941=EDGE_CURVE('',#2419,#2419,#2181,.T.);
#2942=EDGE_CURVE('',#2420,#2420,#2182,.T.);
#2943=EDGE_CURVE('',#2420,#2421,#1264,.T.);
#2944=EDGE_CURVE('',#2421,#2421,#2183,.T.);
#2945=EDGE_CURVE('',#2422,#2422,#2184,.T.);
#2946=EDGE_CURVE('',#2422,#2423,#1265,.T.);
#2947=EDGE_CURVE('',#2423,#2423,#2185,.T.);
#2948=EDGE_CURVE('',#2415,#2424,#1266,.T.);
#2949=EDGE_CURVE('',#2424,#2425,#1267,.T.);
#2950=EDGE_CURVE('',#2425,#2416,#1268,.T.);
#2951=EDGE_CURVE('',#2424,#2426,#2186,.T.);
#2952=EDGE_CURVE('',#2426,#2427,#1269,.T.);
#2953=EDGE_CURVE('',#2427,#2425,#2187,.T.);
#2954=EDGE_CURVE('',#2426,#2428,#1270,.T.);
#2955=EDGE_CURVE('',#2428,#2429,#1271,.T.);
#2956=EDGE_CURVE('',#2429,#2427,#1272,.T.);
#2957=EDGE_CURVE('',#2428,#2430,#2188,.T.);
#2958=EDGE_CURVE('',#2430,#2431,#1273,.T.);
#2959=EDGE_CURVE('',#2431,#2429,#2189,.T.);
#2960=EDGE_CURVE('',#2432,#2430,#1274,.T.);
#2961=EDGE_CURVE('',#2432,#2433,#1275,.T.);
#2962=EDGE_CURVE('',#2433,#2431,#1276,.T.);
#2963=EDGE_CURVE('',#2432,#2434,#2190,.T.);
#2964=EDGE_CURVE('',#2434,#2435,#1277,.T.);
#2965=EDGE_CURVE('',#2435,#2433,#2191,.T.);
#2966=EDGE_CURVE('',#2434,#2414,#1278,.T.);
#2967=EDGE_CURVE('',#2417,#2435,#1279,.T.);
#2968=EDGE_CURVE('',#2436,#2437,#1280,.T.);
#2969=EDGE_CURVE('',#2438,#2437,#1281,.T.);
#2970=EDGE_CURVE('',#2439,#2438,#1282,.T.);
#2971=EDGE_CURVE('',#2439,#2436,#1283,.T.);
#2972=EDGE_CURVE('',#2437,#2440,#1284,.T.);
#2973=EDGE_CURVE('',#2441,#2440,#1285,.T.);
#2974=EDGE_CURVE('',#2438,#2441,#1286,.T.);
#2975=EDGE_CURVE('',#2440,#2442,#1287,.T.);
#2976=EDGE_CURVE('',#2443,#2442,#1288,.T.);
#2977=EDGE_CURVE('',#2441,#2443,#1289,.T.);
#2978=EDGE_CURVE('',#2442,#2444,#1290,.T.);
#2979=EDGE_CURVE('',#2445,#2444,#1291,.T.);
#2980=EDGE_CURVE('',#2443,#2445,#1292,.T.);
#2981=EDGE_CURVE('',#2444,#2446,#1293,.T.);
#2982=EDGE_CURVE('',#2447,#2446,#1294,.T.);
#2983=EDGE_CURVE('',#2445,#2447,#1295,.T.);
#2984=EDGE_CURVE('',#2446,#2436,#1296,.T.);
#2985=EDGE_CURVE('',#2447,#2439,#1297,.T.);
#2986=EDGE_CURVE('',#2448,#2449,#1298,.T.);
#2987=EDGE_CURVE('',#2450,#2449,#1299,.T.);
#2988=EDGE_CURVE('',#2451,#2450,#1300,.T.);
#2989=EDGE_CURVE('',#2451,#2448,#1301,.T.);
#2990=EDGE_CURVE('',#2449,#2452,#1302,.T.);
#2991=EDGE_CURVE('',#2453,#2452,#1303,.T.);
#2992=EDGE_CURVE('',#2450,#2453,#1304,.T.);
#2993=EDGE_CURVE('',#2452,#2454,#1305,.T.);
#2994=EDGE_CURVE('',#2455,#2454,#1306,.T.);
#2995=EDGE_CURVE('',#2453,#2455,#1307,.T.);
#2996=EDGE_CURVE('',#2454,#2456,#1308,.T.);
#2997=EDGE_CURVE('',#2457,#2456,#1309,.T.);
#2998=EDGE_CURVE('',#2455,#2457,#1310,.T.);
#2999=EDGE_CURVE('',#2456,#2458,#1311,.T.);
#3000=EDGE_CURVE('',#2459,#2458,#1312,.T.);
#3001=EDGE_CURVE('',#2457,#2459,#1313,.T.);
#3002=EDGE_CURVE('',#2458,#2448,#1314,.T.);
#3003=EDGE_CURVE('',#2459,#2451,#1315,.T.);
#3004=EDGE_CURVE('',#2460,#2461,#1316,.T.);
#3005=EDGE_CURVE('',#2462,#2461,#1317,.T.);
#3006=EDGE_CURVE('',#2463,#2462,#1318,.T.);
#3007=EDGE_CURVE('',#2463,#2460,#1319,.T.);
#3008=EDGE_CURVE('',#2461,#2464,#1320,.T.);
#3009=EDGE_CURVE('',#2465,#2464,#1321,.T.);
#3010=EDGE_CURVE('',#2462,#2465,#1322,.T.);
#3011=EDGE_CURVE('',#2464,#2466,#1323,.T.);
#3012=EDGE_CURVE('',#2467,#2466,#1324,.T.);
#3013=EDGE_CURVE('',#2465,#2467,#1325,.T.);
#3014=EDGE_CURVE('',#2466,#2468,#1326,.T.);
#3015=EDGE_CURVE('',#2469,#2468,#1327,.T.);
#3016=EDGE_CURVE('',#2467,#2469,#1328,.T.);
#3017=EDGE_CURVE('',#2468,#2470,#1329,.T.);
#3018=EDGE_CURVE('',#2471,#2470,#1330,.T.);
#3019=EDGE_CURVE('',#2469,#2471,#1331,.T.);
#3020=EDGE_CURVE('',#2470,#2460,#1332,.T.);
#3021=EDGE_CURVE('',#2471,#2463,#1333,.T.);
#3022=EDGE_CURVE('',#2472,#2472,#2192,.T.);
#3023=EDGE_CURVE('',#2472,#2473,#1334,.T.);
#3024=EDGE_CURVE('',#2473,#2473,#2193,.T.);
#3025=EDGE_CURVE('',#2474,#2475,#2194,.T.);
#3026=EDGE_CURVE('',#2474,#2476,#1335,.T.);
#3027=EDGE_CURVE('',#2476,#2477,#2195,.T.);
#3028=EDGE_CURVE('',#2475,#2477,#1336,.T.);
#3029=EDGE_CURVE('',#2478,#2478,#2196,.T.);
#3030=EDGE_CURVE('',#2478,#2479,#1337,.T.);
#3031=EDGE_CURVE('',#2479,#2479,#2197,.T.);
#3032=EDGE_CURVE('',#2480,#2480,#2198,.T.);
#3033=EDGE_CURVE('',#2480,#2481,#1338,.T.);
#3034=EDGE_CURVE('',#2481,#2481,#2199,.T.);
#3035=EDGE_CURVE('',#2482,#2482,#2200,.T.);
#3036=EDGE_CURVE('',#2482,#2483,#1339,.T.);
#3037=EDGE_CURVE('',#2483,#2483,#2201,.T.);
#3038=EDGE_CURVE('',#2484,#2485,#1340,.T.);
#3039=EDGE_CURVE('',#2485,#2486,#1341,.T.);
#3040=EDGE_CURVE('',#2486,#2487,#2202,.T.);
#3041=EDGE_CURVE('',#2487,#2488,#1342,.T.);
#3042=EDGE_CURVE('',#2488,#2489,#2203,.T.);
#3043=EDGE_CURVE('',#2489,#2490,#1343,.T.);
#3044=EDGE_CURVE('',#2490,#2491,#1344,.T.);
#3045=EDGE_CURVE('',#2491,#2492,#1345,.T.);
#3046=EDGE_CURVE('',#2492,#2493,#1346,.T.);
#3047=EDGE_CURVE('',#2493,#2494,#1347,.T.);
#3048=EDGE_CURVE('',#2494,#2495,#1348,.T.);
#3049=EDGE_CURVE('',#2495,#2496,#2204,.T.);
#3050=EDGE_CURVE('',#2496,#2497,#1349,.T.);
#3051=EDGE_CURVE('',#2497,#2498,#1350,.T.);
#3052=EDGE_CURVE('',#2498,#2499,#1351,.T.);
#3053=EDGE_CURVE('',#2499,#2500,#1352,.T.);
#3054=EDGE_CURVE('',#2500,#2501,#1353,.T.);
#3055=EDGE_CURVE('',#2501,#2502,#1354,.T.);
#3056=EDGE_CURVE('',#2502,#2503,#1355,.T.);
#3057=EDGE_CURVE('',#2503,#2484,#1356,.T.);
#3058=EDGE_CURVE('',#2504,#2505,#2205,.T.);
#3059=EDGE_CURVE('',#2506,#2504,#1357,.T.);
#3060=EDGE_CURVE('',#2507,#2506,#1358,.T.);
#3061=EDGE_CURVE('',#2508,#2507,#1359,.T.);
#3062=EDGE_CURVE('',#2509,#2508,#1360,.T.);
#3063=EDGE_CURVE('',#2510,#2509,#2206,.T.);
#3064=EDGE_CURVE('',#2511,#2510,#1361,.T.);
#3065=EDGE_CURVE('',#2505,#2511,#1362,.T.);
#3066=EDGE_CURVE('',#2512,#2513,#1363,.T.);
#3067=EDGE_CURVE('',#2514,#2512,#1364,.T.);
#3068=EDGE_CURVE('',#2515,#2514,#1365,.T.);
#3069=EDGE_CURVE('',#2516,#2515,#2207,.T.);
#3070=EDGE_CURVE('',#2513,#2516,#1366,.T.);
#3071=EDGE_CURVE('',#2517,#2518,#1367,.T.);
#3072=EDGE_CURVE('',#2519,#2517,#1368,.T.);
#3073=EDGE_CURVE('',#2520,#2519,#1369,.T.);
#3074=EDGE_CURVE('',#2521,#2520,#1370,.T.);
#3075=EDGE_CURVE('',#2518,#2521,#2208,.T.);
#3076=EDGE_CURVE('',#2522,#2523,#1371,.T.);
#3077=EDGE_CURVE('',#2524,#2522,#1372,.T.);
#3078=EDGE_CURVE('',#2525,#2524,#1373,.T.);
#3079=EDGE_CURVE('',#2526,#2525,#1374,.T.);
#3080=EDGE_CURVE('',#2527,#2526,#1375,.T.);
#3081=EDGE_CURVE('',#2528,#2527,#1376,.T.);
#3082=EDGE_CURVE('',#2529,#2528,#1377,.T.);
#3083=EDGE_CURVE('',#2530,#2529,#1378,.T.);
#3084=EDGE_CURVE('',#2531,#2530,#1379,.T.);
#3085=EDGE_CURVE('',#2532,#2531,#2209,.T.);
#3086=EDGE_CURVE('',#2533,#2532,#1380,.T.);
#3087=EDGE_CURVE('',#2534,#2533,#1381,.T.);
#3088=EDGE_CURVE('',#2535,#2534,#1382,.T.);
#3089=EDGE_CURVE('',#2536,#2535,#1383,.T.);
#3090=EDGE_CURVE('',#2537,#2536,#1384,.T.);
#3091=EDGE_CURVE('',#2538,#2537,#1385,.T.);
#3092=EDGE_CURVE('',#2539,#2538,#2210,.T.);
#3093=EDGE_CURVE('',#2540,#2539,#1386,.T.);
#3094=EDGE_CURVE('',#2541,#2540,#2211,.T.);
#3095=EDGE_CURVE('',#2523,#2541,#1387,.T.);
#3096=EDGE_CURVE('',#2542,#2543,#1388,.T.);
#3097=EDGE_CURVE('',#2544,#2542,#1389,.T.);
#3098=EDGE_CURVE('',#2545,#2544,#1390,.T.);
#3099=EDGE_CURVE('',#2546,#2545,#1391,.T.);
#3100=EDGE_CURVE('',#2543,#2546,#2212,.T.);
#3101=EDGE_CURVE('',#2547,#2548,#1392,.T.);
#3102=EDGE_CURVE('',#2549,#2547,#1393,.T.);
#3103=EDGE_CURVE('',#2550,#2549,#1394,.T.);
#3104=EDGE_CURVE('',#2551,#2550,#2213,.T.);
#3105=EDGE_CURVE('',#2548,#2551,#1395,.T.);
#3106=EDGE_CURVE('',#2552,#2476,#1396,.T.);
#3107=EDGE_CURVE('',#2553,#2552,#1397,.T.);
#3108=EDGE_CURVE('',#2554,#2553,#2214,.T.);
#3109=EDGE_CURVE('',#2555,#2554,#1398,.T.);
#3110=EDGE_CURVE('',#2556,#2555,#1399,.T.);
#3111=EDGE_CURVE('',#2557,#2556,#1400,.T.);
#3112=EDGE_CURVE('',#2477,#2557,#1401,.T.);
#3113=EDGE_CURVE('',#2485,#2523,#1402,.T.);
#3114=EDGE_CURVE('',#2484,#2522,#1403,.T.);
#3115=EDGE_CURVE('',#2486,#2541,#1404,.T.);
#3116=EDGE_CURVE('',#2487,#2540,#1405,.T.);
#3117=EDGE_CURVE('',#2488,#2539,#1406,.T.);
#3118=EDGE_CURVE('',#2489,#2538,#1407,.T.);
#3119=EDGE_CURVE('',#2490,#2537,#1408,.T.);
#3120=EDGE_CURVE('',#2491,#2536,#1409,.T.);
#3121=EDGE_CURVE('',#2492,#2535,#1410,.T.);
#3122=EDGE_CURVE('',#2493,#2534,#1411,.T.);
#3123=EDGE_CURVE('',#2494,#2533,#1412,.T.);
#3124=EDGE_CURVE('',#2495,#2532,#1413,.T.);
#3125=EDGE_CURVE('',#2496,#2531,#1414,.T.);
#3126=EDGE_CURVE('',#2497,#2530,#1415,.T.);
#3127=EDGE_CURVE('',#2498,#2529,#1416,.T.);
#3128=EDGE_CURVE('',#2499,#2528,#1417,.T.);
#3129=EDGE_CURVE('',#2500,#2527,#1418,.T.);
#3130=EDGE_CURVE('',#2501,#2526,#1419,.T.);
#3131=EDGE_CURVE('',#2502,#2525,#1420,.T.);
#3132=EDGE_CURVE('',#2503,#2524,#1421,.T.);
#3133=EDGE_CURVE('',#2558,#2518,#1422,.T.);
#3134=EDGE_CURVE('',#2559,#2558,#1423,.T.);
#3135=EDGE_CURVE('',#2559,#2517,#1424,.T.);
#3136=EDGE_CURVE('',#2560,#2559,#1425,.T.);
#3137=EDGE_CURVE('',#2560,#2519,#1426,.T.);
#3138=EDGE_CURVE('',#2561,#2560,#1427,.T.);
#3139=EDGE_CURVE('',#2561,#2520,#1428,.T.);
#3140=EDGE_CURVE('',#2562,#2561,#1429,.T.);
#3141=EDGE_CURVE('',#2562,#2521,#1430,.T.);
#3142=EDGE_CURVE('',#2558,#2562,#2215,.T.);
#3143=EDGE_CURVE('',#2563,#2513,#1431,.T.);
#3144=EDGE_CURVE('',#2564,#2563,#1432,.T.);
#3145=EDGE_CURVE('',#2564,#2512,#1433,.T.);
#3146=EDGE_CURVE('',#2565,#2564,#1434,.T.);
#3147=EDGE_CURVE('',#2565,#2514,#1435,.T.);
#3148=EDGE_CURVE('',#2566,#2565,#1436,.T.);
#3149=EDGE_CURVE('',#2566,#2515,#1437,.T.);
#3150=EDGE_CURVE('',#2567,#2566,#2216,.T.);
#3151=EDGE_CURVE('',#2567,#2516,#1438,.T.);
#3152=EDGE_CURVE('',#2563,#2567,#1439,.T.);
#3153=EDGE_CURVE('',#2568,#2505,#1440,.T.);
#3154=EDGE_CURVE('',#2569,#2568,#2217,.T.);
#3155=EDGE_CURVE('',#2569,#2504,#1441,.T.);
#3156=EDGE_CURVE('',#2570,#2569,#1442,.T.);
#3157=EDGE_CURVE('',#2570,#2506,#1443,.T.);
#3158=EDGE_CURVE('',#2571,#2570,#1444,.T.);
#3159=EDGE_CURVE('',#2571,#2507,#1445,.T.);
#3160=EDGE_CURVE('',#2572,#2571,#1446,.T.);
#3161=EDGE_CURVE('',#2572,#2508,#1447,.T.);
#3162=EDGE_CURVE('',#2573,#2572,#1448,.T.);
#3163=EDGE_CURVE('',#2573,#2509,#1449,.T.);
#3164=EDGE_CURVE('',#2574,#2573,#2218,.T.);
#3165=EDGE_CURVE('',#2574,#2510,#1450,.T.);
#3166=EDGE_CURVE('',#2575,#2574,#1451,.T.);
#3167=EDGE_CURVE('',#2575,#2511,#1452,.T.);
#3168=EDGE_CURVE('',#2568,#2575,#1453,.T.);
#3169=EDGE_CURVE('',#2576,#2474,#1454,.T.);
#3170=EDGE_CURVE('',#2576,#2552,#1455,.T.);
#3171=EDGE_CURVE('',#2577,#2576,#1456,.T.);
#3172=EDGE_CURVE('',#2577,#2553,#1457,.T.);
#3173=EDGE_CURVE('',#2578,#2577,#2219,.T.);
#3174=EDGE_CURVE('',#2578,#2554,#1458,.T.);
#3175=EDGE_CURVE('',#2579,#2578,#1459,.T.);
#3176=EDGE_CURVE('',#2579,#2555,#1460,.T.);
#3177=EDGE_CURVE('',#2580,#2579,#1461,.T.);
#3178=EDGE_CURVE('',#2580,#2556,#1462,.T.);
#3179=EDGE_CURVE('',#2581,#2580,#1463,.T.);
#3180=EDGE_CURVE('',#2581,#2557,#1464,.T.);
#3181=EDGE_CURVE('',#2475,#2581,#1465,.T.);
#3182=EDGE_CURVE('',#2582,#2547,#1466,.T.);
#3183=EDGE_CURVE('',#2583,#2582,#1467,.T.);
#3184=EDGE_CURVE('',#2583,#2549,#1468,.T.);
#3185=EDGE_CURVE('',#2584,#2583,#1469,.T.);
#3186=EDGE_CURVE('',#2584,#2550,#1470,.T.);
#3187=EDGE_CURVE('',#2585,#2584,#2220,.T.);
#3188=EDGE_CURVE('',#2585,#2551,#1471,.T.);
#3189=EDGE_CURVE('',#2586,#2585,#1472,.T.);
#3190=EDGE_CURVE('',#2586,#2548,#1473,.T.);
#3191=EDGE_CURVE('',#2582,#2586,#1474,.T.);
#3192=EDGE_CURVE('',#2587,#2542,#1475,.T.);
#3193=EDGE_CURVE('',#2588,#2587,#1476,.T.);
#3194=EDGE_CURVE('',#2588,#2544,#1477,.T.);
#3195=EDGE_CURVE('',#2589,#2588,#1478,.T.);
#3196=EDGE_CURVE('',#2589,#2545,#1479,.T.);
#3197=EDGE_CURVE('',#2590,#2589,#1480,.T.);
#3198=EDGE_CURVE('',#2590,#2546,#1481,.T.);
#3199=EDGE_CURVE('',#2591,#2590,#2221,.T.);
#3200=EDGE_CURVE('',#2591,#2543,#1482,.T.);
#3201=EDGE_CURVE('',#2587,#2591,#1483,.T.);
#3202=EDGE_CURVE('',#2592,#2592,#2222,.T.);
#3203=EDGE_CURVE('',#2592,#2593,#1484,.T.);
#3204=EDGE_CURVE('',#2593,#2593,#2223,.T.);
#3205=EDGE_CURVE('',#2594,#2594,#2224,.T.);
#3206=EDGE_CURVE('',#2594,#2595,#1485,.T.);
#3207=EDGE_CURVE('',#2595,#2595,#2225,.T.);
#3208=EDGE_CURVE('',#2596,#2596,#2226,.T.);
#3209=EDGE_CURVE('',#2596,#2597,#1486,.T.);
#3210=EDGE_CURVE('',#2597,#2597,#2227,.T.);
#3211=EDGE_CURVE('',#2598,#2598,#2228,.T.);
#3212=EDGE_CURVE('',#2598,#2599,#1487,.T.);
#3213=EDGE_CURVE('',#2599,#2599,#2229,.T.);
#3214=EDGE_CURVE('',#2600,#2600,#2230,.T.);
#3215=EDGE_CURVE('',#2600,#2601,#1488,.T.);
#3216=EDGE_CURVE('',#2601,#2601,#2231,.T.);
#3217=EDGE_CURVE('',#2602,#2603,#2232,.T.);
#3218=EDGE_CURVE('',#2602,#2604,#1489,.T.);
#3219=EDGE_CURVE('',#2604,#2605,#2233,.T.);
#3220=EDGE_CURVE('',#2603,#2605,#1490,.T.);
#3221=EDGE_CURVE('',#2606,#2607,#207,.T.);
#3222=EDGE_CURVE('',#2607,#2608,#2234,.T.);
#3223=EDGE_CURVE('',#2608,#2609,#208,.T.);
#3224=EDGE_CURVE('',#2609,#2610,#2235,.T.);
#3225=EDGE_CURVE('',#2610,#2611,#209,.T.);
#3226=EDGE_CURVE('',#2611,#2612,#2236,.T.);
#3227=EDGE_CURVE('',#2612,#2613,#210,.T.);
#3228=EDGE_CURVE('',#2613,#2614,#2237,.T.);
#3229=EDGE_CURVE('',#2614,#2615,#211,.T.);
#3230=EDGE_CURVE('',#2615,#2616,#2238,.T.);
#3231=EDGE_CURVE('',#2616,#2617,#212,.T.);
#3232=EDGE_CURVE('',#2617,#2618,#2239,.T.);
#3233=EDGE_CURVE('',#2618,#2619,#213,.T.);
#3234=EDGE_CURVE('',#2619,#2620,#2240,.T.);
#3235=EDGE_CURVE('',#2620,#2621,#214,.T.);
#3236=EDGE_CURVE('',#2621,#2622,#2241,.T.);
#3237=EDGE_CURVE('',#2622,#2623,#215,.T.);
#3238=EDGE_CURVE('',#2623,#2624,#2242,.T.);
#3239=EDGE_CURVE('',#2624,#2625,#216,.T.);
#3240=EDGE_CURVE('',#2625,#2626,#2243,.T.);
#3241=EDGE_CURVE('',#2626,#2627,#217,.T.);
#3242=EDGE_CURVE('',#2627,#2628,#2244,.T.);
#3243=EDGE_CURVE('',#2628,#2629,#218,.T.);
#3244=EDGE_CURVE('',#2629,#2630,#2245,.T.);
#3245=EDGE_CURVE('',#2630,#2631,#219,.T.);
#3246=EDGE_CURVE('',#2631,#2632,#2246,.T.);
#3247=EDGE_CURVE('',#2632,#2633,#220,.T.);
#3248=EDGE_CURVE('',#2633,#2634,#2247,.T.);
#3249=EDGE_CURVE('',#2634,#2635,#221,.T.);
#3250=EDGE_CURVE('',#2635,#2636,#2248,.T.);
#3251=EDGE_CURVE('',#2636,#2637,#222,.T.);
#3252=EDGE_CURVE('',#2637,#2638,#2249,.T.);
#3253=EDGE_CURVE('',#2638,#2639,#223,.T.);
#3254=EDGE_CURVE('',#2639,#2640,#2250,.T.);
#3255=EDGE_CURVE('',#2640,#2602,#224,.T.);
#3256=EDGE_CURVE('',#2603,#2641,#225,.T.);
#3257=EDGE_CURVE('',#2641,#2642,#2251,.T.);
#3258=EDGE_CURVE('',#2642,#2643,#226,.T.);
#3259=EDGE_CURVE('',#2643,#2644,#2252,.T.);
#3260=EDGE_CURVE('',#2644,#2645,#227,.T.);
#3261=EDGE_CURVE('',#2645,#2646,#2253,.T.);
#3262=EDGE_CURVE('',#2646,#2647,#228,.T.);
#3263=EDGE_CURVE('',#2647,#2648,#2254,.T.);
#3264=EDGE_CURVE('',#2648,#2649,#229,.T.);
#3265=EDGE_CURVE('',#2649,#2650,#2255,.T.);
#3266=EDGE_CURVE('',#2650,#2651,#230,.T.);
#3267=EDGE_CURVE('',#2651,#2652,#2256,.T.);
#3268=EDGE_CURVE('',#2652,#2653,#231,.T.);
#3269=EDGE_CURVE('',#2653,#2654,#2257,.T.);
#3270=EDGE_CURVE('',#2654,#2655,#232,.T.);
#3271=EDGE_CURVE('',#2655,#2656,#2258,.T.);
#3272=EDGE_CURVE('',#2656,#2657,#233,.T.);
#3273=EDGE_CURVE('',#2657,#2658,#2259,.T.);
#3274=EDGE_CURVE('',#2658,#2659,#234,.T.);
#3275=EDGE_CURVE('',#2659,#2660,#2260,.T.);
#3276=EDGE_CURVE('',#2660,#2661,#235,.T.);
#3277=EDGE_CURVE('',#2661,#2662,#2261,.T.);
#3278=EDGE_CURVE('',#2662,#2663,#236,.T.);
#3279=EDGE_CURVE('',#2663,#2664,#2262,.T.);
#3280=EDGE_CURVE('',#2664,#2665,#237,.T.);
#3281=EDGE_CURVE('',#2665,#2666,#2263,.T.);
#3282=EDGE_CURVE('',#2666,#2667,#238,.T.);
#3283=EDGE_CURVE('',#2667,#2668,#2264,.T.);
#3284=EDGE_CURVE('',#2668,#2669,#239,.T.);
#3285=EDGE_CURVE('',#2669,#2670,#2265,.T.);
#3286=EDGE_CURVE('',#2670,#2671,#240,.T.);
#3287=EDGE_CURVE('',#2671,#2672,#2266,.T.);
#3288=EDGE_CURVE('',#2672,#2673,#241,.T.);
#3289=EDGE_CURVE('',#2673,#2674,#2267,.T.);
#3290=EDGE_CURVE('',#2674,#2675,#242,.T.);
#3291=EDGE_CURVE('',#2675,#2676,#2268,.T.);
#3292=EDGE_CURVE('',#2676,#2677,#243,.T.);
#3293=EDGE_CURVE('',#2677,#2678,#2269,.T.);
#3294=EDGE_CURVE('',#2678,#2679,#244,.T.);
#3295=EDGE_CURVE('',#2679,#2680,#2270,.T.);
#3296=EDGE_CURVE('',#2680,#2681,#245,.T.);
#3297=EDGE_CURVE('',#2681,#2682,#2271,.T.);
#3298=EDGE_CURVE('',#2682,#2683,#246,.T.);
#3299=EDGE_CURVE('',#2683,#2606,#2272,.T.);
#3300=EDGE_CURVE('',#2684,#2685,#247,.T.);
#3301=EDGE_CURVE('',#2686,#2684,#2273,.T.);
#3302=EDGE_CURVE('',#2687,#2686,#248,.T.);
#3303=EDGE_CURVE('',#2688,#2687,#2274,.T.);
#3304=EDGE_CURVE('',#2689,#2688,#249,.T.);
#3305=EDGE_CURVE('',#2690,#2689,#2275,.T.);
#3306=EDGE_CURVE('',#2691,#2690,#250,.T.);
#3307=EDGE_CURVE('',#2692,#2691,#2276,.T.);
#3308=EDGE_CURVE('',#2693,#2692,#251,.T.);
#3309=EDGE_CURVE('',#2694,#2693,#2277,.T.);
#3310=EDGE_CURVE('',#2695,#2694,#252,.T.);
#3311=EDGE_CURVE('',#2696,#2695,#2278,.T.);
#3312=EDGE_CURVE('',#2697,#2696,#253,.T.);
#3313=EDGE_CURVE('',#2698,#2697,#2279,.T.);
#3314=EDGE_CURVE('',#2699,#2698,#254,.T.);
#3315=EDGE_CURVE('',#2700,#2699,#2280,.T.);
#3316=EDGE_CURVE('',#2701,#2700,#255,.T.);
#3317=EDGE_CURVE('',#2702,#2701,#2281,.T.);
#3318=EDGE_CURVE('',#2703,#2702,#256,.T.);
#3319=EDGE_CURVE('',#2704,#2703,#2282,.T.);
#3320=EDGE_CURVE('',#2705,#2704,#257,.T.);
#3321=EDGE_CURVE('',#2706,#2705,#2283,.T.);
#3322=EDGE_CURVE('',#2707,#2706,#258,.T.);
#3323=EDGE_CURVE('',#2708,#2707,#2284,.T.);
#3324=EDGE_CURVE('',#2709,#2708,#259,.T.);
#3325=EDGE_CURVE('',#2710,#2709,#2285,.T.);
#3326=EDGE_CURVE('',#2711,#2710,#260,.T.);
#3327=EDGE_CURVE('',#2712,#2711,#2286,.T.);
#3328=EDGE_CURVE('',#2713,#2712,#261,.T.);
#3329=EDGE_CURVE('',#2714,#2713,#2287,.T.);
#3330=EDGE_CURVE('',#2715,#2714,#262,.T.);
#3331=EDGE_CURVE('',#2716,#2715,#2288,.T.);
#3332=EDGE_CURVE('',#2717,#2716,#263,.T.);
#3333=EDGE_CURVE('',#2718,#2717,#2289,.T.);
#3334=EDGE_CURVE('',#2719,#2718,#264,.T.);
#3335=EDGE_CURVE('',#2720,#2719,#2290,.T.);
#3336=EDGE_CURVE('',#2721,#2720,#265,.T.);
#3337=EDGE_CURVE('',#2722,#2721,#2291,.T.);
#3338=EDGE_CURVE('',#2723,#2722,#266,.T.);
#3339=EDGE_CURVE('',#2724,#2723,#2292,.T.);
#3340=EDGE_CURVE('',#2725,#2724,#267,.T.);
#3341=EDGE_CURVE('',#2726,#2725,#2293,.T.);
#3342=EDGE_CURVE('',#2727,#2726,#268,.T.);
#3343=EDGE_CURVE('',#2728,#2727,#2294,.T.);
#3344=EDGE_CURVE('',#2605,#2728,#269,.T.);
#3345=EDGE_CURVE('',#2729,#2604,#270,.T.);
#3346=EDGE_CURVE('',#2730,#2729,#2295,.T.);
#3347=EDGE_CURVE('',#2731,#2730,#271,.T.);
#3348=EDGE_CURVE('',#2732,#2731,#2296,.T.);
#3349=EDGE_CURVE('',#2733,#2732,#272,.T.);
#3350=EDGE_CURVE('',#2734,#2733,#2297,.T.);
#3351=EDGE_CURVE('',#2735,#2734,#273,.T.);
#3352=EDGE_CURVE('',#2736,#2735,#2298,.T.);
#3353=EDGE_CURVE('',#2737,#2736,#274,.T.);
#3354=EDGE_CURVE('',#2738,#2737,#2299,.T.);
#3355=EDGE_CURVE('',#2739,#2738,#275,.T.);
#3356=EDGE_CURVE('',#2740,#2739,#2300,.T.);
#3357=EDGE_CURVE('',#2741,#2740,#276,.T.);
#3358=EDGE_CURVE('',#2742,#2741,#2301,.T.);
#3359=EDGE_CURVE('',#2743,#2742,#277,.T.);
#3360=EDGE_CURVE('',#2744,#2743,#2302,.T.);
#3361=EDGE_CURVE('',#2745,#2744,#278,.T.);
#3362=EDGE_CURVE('',#2746,#2745,#2303,.T.);
#3363=EDGE_CURVE('',#2747,#2746,#279,.T.);
#3364=EDGE_CURVE('',#2748,#2747,#2304,.T.);
#3365=EDGE_CURVE('',#2749,#2748,#280,.T.);
#3366=EDGE_CURVE('',#2750,#2749,#2305,.T.);
#3367=EDGE_CURVE('',#2751,#2750,#281,.T.);
#3368=EDGE_CURVE('',#2752,#2751,#2306,.T.);
#3369=EDGE_CURVE('',#2753,#2752,#282,.T.);
#3370=EDGE_CURVE('',#2754,#2753,#2307,.T.);
#3371=EDGE_CURVE('',#2755,#2754,#283,.T.);
#3372=EDGE_CURVE('',#2756,#2755,#2308,.T.);
#3373=EDGE_CURVE('',#2757,#2756,#284,.T.);
#3374=EDGE_CURVE('',#2758,#2757,#2309,.T.);
#3375=EDGE_CURVE('',#2759,#2758,#285,.T.);
#3376=EDGE_CURVE('',#2760,#2759,#2310,.T.);
#3377=EDGE_CURVE('',#2761,#2760,#286,.T.);
#3378=EDGE_CURVE('',#2685,#2761,#2311,.T.);
#3379=EDGE_CURVE('',#2607,#2685,#1491,.T.);
#3380=EDGE_CURVE('',#2606,#2684,#1492,.T.);
#3381=EDGE_CURVE('',#2608,#2761,#1493,.T.);
#3382=EDGE_CURVE('',#2609,#2760,#1494,.T.);
#3383=EDGE_CURVE('',#2610,#2759,#1495,.T.);
#3384=EDGE_CURVE('',#2611,#2758,#1496,.T.);
#3385=EDGE_CURVE('',#2612,#2757,#1497,.T.);
#3386=EDGE_CURVE('',#2613,#2756,#1498,.T.);
#3387=EDGE_CURVE('',#2614,#2755,#1499,.T.);
#3388=EDGE_CURVE('',#2615,#2754,#1500,.T.);
#3389=EDGE_CURVE('',#2616,#2753,#1501,.T.);
#3390=EDGE_CURVE('',#2617,#2752,#1502,.T.);
#3391=EDGE_CURVE('',#2618,#2751,#1503,.T.);
#3392=EDGE_CURVE('',#2619,#2750,#1504,.T.);
#3393=EDGE_CURVE('',#2620,#2749,#1505,.T.);
#3394=EDGE_CURVE('',#2621,#2748,#1506,.T.);
#3395=EDGE_CURVE('',#2622,#2747,#1507,.T.);
#3396=EDGE_CURVE('',#2623,#2746,#1508,.T.);
#3397=EDGE_CURVE('',#2624,#2745,#1509,.T.);
#3398=EDGE_CURVE('',#2625,#2744,#1510,.T.);
#3399=EDGE_CURVE('',#2626,#2743,#1511,.T.);
#3400=EDGE_CURVE('',#2627,#2742,#1512,.T.);
#3401=EDGE_CURVE('',#2628,#2741,#1513,.T.);
#3402=EDGE_CURVE('',#2629,#2740,#1514,.T.);
#3403=EDGE_CURVE('',#2630,#2739,#1515,.T.);
#3404=EDGE_CURVE('',#2631,#2738,#1516,.T.);
#3405=EDGE_CURVE('',#2632,#2737,#1517,.T.);
#3406=EDGE_CURVE('',#2633,#2736,#1518,.T.);
#3407=EDGE_CURVE('',#2634,#2735,#1519,.T.);
#3408=EDGE_CURVE('',#2635,#2734,#1520,.T.);
#3409=EDGE_CURVE('',#2636,#2733,#1521,.T.);
#3410=EDGE_CURVE('',#2637,#2732,#1522,.T.);
#3411=EDGE_CURVE('',#2638,#2731,#1523,.T.);
#3412=EDGE_CURVE('',#2639,#2730,#1524,.T.);
#3413=EDGE_CURVE('',#2640,#2729,#1525,.T.);
#3414=EDGE_CURVE('',#2641,#2728,#1526,.T.);
#3415=EDGE_CURVE('',#2642,#2727,#1527,.T.);
#3416=EDGE_CURVE('',#2643,#2726,#1528,.T.);
#3417=EDGE_CURVE('',#2644,#2725,#1529,.T.);
#3418=EDGE_CURVE('',#2645,#2724,#1530,.T.);
#3419=EDGE_CURVE('',#2646,#2723,#1531,.T.);
#3420=EDGE_CURVE('',#2647,#2722,#1532,.T.);
#3421=EDGE_CURVE('',#2648,#2721,#1533,.T.);
#3422=EDGE_CURVE('',#2649,#2720,#1534,.T.);
#3423=EDGE_CURVE('',#2650,#2719,#1535,.T.);
#3424=EDGE_CURVE('',#2651,#2718,#1536,.T.);
#3425=EDGE_CURVE('',#2652,#2717,#1537,.T.);
#3426=EDGE_CURVE('',#2653,#2716,#1538,.T.);
#3427=EDGE_CURVE('',#2654,#2715,#1539,.T.);
#3428=EDGE_CURVE('',#2655,#2714,#1540,.T.);
#3429=EDGE_CURVE('',#2656,#2713,#1541,.T.);
#3430=EDGE_CURVE('',#2657,#2712,#1542,.T.);
#3431=EDGE_CURVE('',#2658,#2711,#1543,.T.);
#3432=EDGE_CURVE('',#2659,#2710,#1544,.T.);
#3433=EDGE_CURVE('',#2660,#2709,#1545,.T.);
#3434=EDGE_CURVE('',#2661,#2708,#1546,.T.);
#3435=EDGE_CURVE('',#2662,#2707,#1547,.T.);
#3436=EDGE_CURVE('',#2663,#2706,#1548,.T.);
#3437=EDGE_CURVE('',#2664,#2705,#1549,.T.);
#3438=EDGE_CURVE('',#2665,#2704,#1550,.T.);
#3439=EDGE_CURVE('',#2666,#2703,#1551,.T.);
#3440=EDGE_CURVE('',#2667,#2702,#1552,.T.);
#3441=EDGE_CURVE('',#2668,#2701,#1553,.T.);
#3442=EDGE_CURVE('',#2669,#2700,#1554,.T.);
#3443=EDGE_CURVE('',#2670,#2699,#1555,.T.);
#3444=EDGE_CURVE('',#2671,#2698,#1556,.T.);
#3445=EDGE_CURVE('',#2672,#2697,#1557,.T.);
#3446=EDGE_CURVE('',#2673,#2696,#1558,.T.);
#3447=EDGE_CURVE('',#2674,#2695,#1559,.T.);
#3448=EDGE_CURVE('',#2675,#2694,#1560,.T.);
#3449=EDGE_CURVE('',#2676,#2693,#1561,.T.);
#3450=EDGE_CURVE('',#2677,#2692,#1562,.T.);
#3451=EDGE_CURVE('',#2678,#2691,#1563,.T.);
#3452=EDGE_CURVE('',#2679,#2690,#1564,.T.);
#3453=EDGE_CURVE('',#2680,#2689,#1565,.T.);
#3454=EDGE_CURVE('',#2681,#2688,#1566,.T.);
#3455=EDGE_CURVE('',#2682,#2687,#1567,.T.);
#3456=EDGE_CURVE('',#2683,#2686,#1568,.T.);
#3457=EDGE_CURVE('',#2762,#2762,#2312,.T.);
#3458=EDGE_CURVE('',#2762,#2763,#1569,.T.);
#3459=EDGE_CURVE('',#2763,#2763,#2313,.T.);
#3460=EDGE_CURVE('',#2764,#2764,#2314,.T.);
#3461=EDGE_CURVE('',#2764,#2765,#1570,.T.);
#3462=EDGE_CURVE('',#2765,#2765,#2315,.T.);
#3463=EDGE_CURVE('',#2766,#2767,#2316,.T.);
#3464=EDGE_CURVE('',#2767,#2768,#1571,.T.);
#3465=EDGE_CURVE('',#2768,#2769,#2317,.T.);
#3466=EDGE_CURVE('',#2769,#2766,#1572,.T.);
#3467=EDGE_CURVE('',#2770,#2771,#2318,.T.);
#3468=EDGE_CURVE('',#2772,#2770,#1573,.T.);
#3469=EDGE_CURVE('',#2773,#2772,#2319,.T.);
#3470=EDGE_CURVE('',#2771,#2773,#1574,.T.);
#3471=EDGE_CURVE('',#2767,#2771,#1575,.T.);
#3472=EDGE_CURVE('',#2766,#2770,#1576,.T.);
#3473=EDGE_CURVE('',#2768,#2773,#1577,.T.);
#3474=EDGE_CURVE('',#2769,#2772,#1578,.T.);
#3475=EDGE_CURVE('',#2774,#2775,#1579,.T.);
#3476=EDGE_CURVE('',#2775,#2776,#2320,.T.);
#3477=EDGE_CURVE('',#2776,#2777,#2321,.T.);
#3478=EDGE_CURVE('',#2777,#2778,#2322,.T.);
#3479=EDGE_CURVE('',#2778,#2779,#2323,.T.);
#3480=EDGE_CURVE('',#2779,#2780,#2324,.T.);
#3481=EDGE_CURVE('',#2780,#2775,#2325,.T.);
#3482=EDGE_CURVE('',#2781,#2781,#2326,.T.);
#3483=EDGE_CURVE('',#2781,#2782,#2327,.T.);
#3484=EDGE_CURVE('',#2782,#2782,#2328,.T.);
#3485=EDGE_CURVE('',#2783,#2783,#2329,.T.);
#3486=EDGE_CURVE('',#2783,#2784,#1580,.T.);
#3487=EDGE_CURVE('',#2784,#2784,#2330,.T.);
#3488=EDGE_CURVE('',#2782,#2783,#1581,.T.);
#3489=EDGE_CURVE('',#2785,#2785,#2331,.T.);
#3490=EDGE_CURVE('',#2785,#2786,#1582,.T.);
#3491=EDGE_CURVE('',#2786,#2786,#2332,.T.);
#3492=EDGE_CURVE('',#2787,#2787,#2333,.T.);
#3493=EDGE_CURVE('',#2788,#2789,#1583,.T.);
#3494=EDGE_CURVE('',#2789,#2790,#1584,.T.);
#3495=EDGE_CURVE('',#2790,#2791,#1585,.T.);
#3496=EDGE_CURVE('',#2791,#2792,#1586,.T.);
#3497=EDGE_CURVE('',#2792,#2793,#1587,.T.);
#3498=EDGE_CURVE('',#2793,#2788,#1588,.T.);
#3499=EDGE_CURVE('',#2794,#2777,#1589,.T.);
#3500=EDGE_CURVE('',#2777,#2795,#1590,.T.);
#3501=EDGE_CURVE('',#2795,#2790,#1591,.T.);
#3502=EDGE_CURVE('',#2794,#2789,#1592,.T.);
#3503=EDGE_CURVE('',#2795,#2776,#1593,.T.);
#3504=EDGE_CURVE('',#2776,#2796,#1594,.T.);
#3505=EDGE_CURVE('',#2796,#2791,#1595,.T.);
#3506=EDGE_CURVE('',#2796,#2775,#1596,.T.);
#3507=EDGE_CURVE('',#2775,#2797,#1597,.T.);
#3508=EDGE_CURVE('',#2797,#2792,#1598,.T.);
#3509=EDGE_CURVE('',#2797,#2780,#1599,.T.);
#3510=EDGE_CURVE('',#2780,#2798,#1600,.T.);
#3511=EDGE_CURVE('',#2798,#2793,#1601,.T.);
#3512=EDGE_CURVE('',#2798,#2779,#1602,.T.);
#3513=EDGE_CURVE('',#2779,#2799,#1603,.T.);
#3514=EDGE_CURVE('',#2799,#2788,#1604,.T.);
#3515=EDGE_CURVE('',#2799,#2778,#1605,.T.);
#3516=EDGE_CURVE('',#2778,#2794,#1606,.T.);
#3517=EDGE_CURVE('',#2800,#2801,#1607,.T.);
#3518=EDGE_CURVE('',#2801,#2802,#2334,.T.);
#3519=EDGE_CURVE('',#2802,#2803,#2335,.T.);
#3520=EDGE_CURVE('',#2803,#2804,#2336,.T.);
#3521=EDGE_CURVE('',#2804,#2805,#2337,.T.);
#3522=EDGE_CURVE('',#2805,#2806,#2338,.T.);
#3523=EDGE_CURVE('',#2806,#2801,#2339,.T.);
#3524=EDGE_CURVE('',#2807,#2807,#2340,.T.);
#3525=EDGE_CURVE('',#2807,#2808,#2341,.T.);
#3526=EDGE_CURVE('',#2808,#2808,#2342,.T.);
#3527=EDGE_CURVE('',#2809,#2809,#2343,.T.);
#3528=EDGE_CURVE('',#2809,#2810,#1608,.T.);
#3529=EDGE_CURVE('',#2810,#2810,#2344,.T.);
#3530=EDGE_CURVE('',#2808,#2809,#1609,.T.);
#3531=EDGE_CURVE('',#2811,#2811,#2345,.T.);
#3532=EDGE_CURVE('',#2811,#2812,#1610,.T.);
#3533=EDGE_CURVE('',#2812,#2812,#2346,.T.);
#3534=EDGE_CURVE('',#2813,#2813,#2347,.T.);
#3535=EDGE_CURVE('',#2814,#2815,#1611,.T.);
#3536=EDGE_CURVE('',#2815,#2816,#1612,.T.);
#3537=EDGE_CURVE('',#2816,#2817,#1613,.T.);
#3538=EDGE_CURVE('',#2817,#2818,#1614,.T.);
#3539=EDGE_CURVE('',#2818,#2819,#1615,.T.);
#3540=EDGE_CURVE('',#2819,#2814,#1616,.T.);
#3541=EDGE_CURVE('',#2820,#2803,#1617,.T.);
#3542=EDGE_CURVE('',#2803,#2821,#1618,.T.);
#3543=EDGE_CURVE('',#2821,#2816,#1619,.T.);
#3544=EDGE_CURVE('',#2820,#2815,#1620,.T.);
#3545=EDGE_CURVE('',#2821,#2802,#1621,.T.);
#3546=EDGE_CURVE('',#2802,#2822,#1622,.T.);
#3547=EDGE_CURVE('',#2822,#2817,#1623,.T.);
#3548=EDGE_CURVE('',#2822,#2801,#1624,.T.);
#3549=EDGE_CURVE('',#2801,#2823,#1625,.T.);
#3550=EDGE_CURVE('',#2823,#2818,#1626,.T.);
#3551=EDGE_CURVE('',#2823,#2806,#1627,.T.);
#3552=EDGE_CURVE('',#2806,#2824,#1628,.T.);
#3553=EDGE_CURVE('',#2824,#2819,#1629,.T.);
#3554=EDGE_CURVE('',#2824,#2805,#1630,.T.);
#3555=EDGE_CURVE('',#2805,#2825,#1631,.T.);
#3556=EDGE_CURVE('',#2825,#2814,#1632,.T.);
#3557=EDGE_CURVE('',#2825,#2804,#1633,.T.);
#3558=EDGE_CURVE('',#2804,#2820,#1634,.T.);
#3559=EDGE_CURVE('',#2826,#2827,#1635,.T.);
#3560=EDGE_CURVE('',#2827,#2828,#2348,.T.);
#3561=EDGE_CURVE('',#2828,#2829,#2349,.T.);
#3562=EDGE_CURVE('',#2829,#2830,#2350,.T.);
#3563=EDGE_CURVE('',#2830,#2831,#2351,.T.);
#3564=EDGE_CURVE('',#2831,#2832,#2352,.T.);
#3565=EDGE_CURVE('',#2832,#2827,#2353,.T.);
#3566=EDGE_CURVE('',#2833,#2833,#2354,.T.);
#3567=EDGE_CURVE('',#2833,#2834,#2355,.T.);
#3568=EDGE_CURVE('',#2834,#2834,#2356,.T.);
#3569=EDGE_CURVE('',#2835,#2835,#2357,.T.);
#3570=EDGE_CURVE('',#2835,#2836,#1636,.T.);
#3571=EDGE_CURVE('',#2836,#2836,#2358,.T.);
#3572=EDGE_CURVE('',#2834,#2835,#1637,.T.);
#3573=EDGE_CURVE('',#2837,#2837,#2359,.T.);
#3574=EDGE_CURVE('',#2837,#2838,#1638,.T.);
#3575=EDGE_CURVE('',#2838,#2838,#2360,.T.);
#3576=EDGE_CURVE('',#2839,#2839,#2361,.T.);
#3577=EDGE_CURVE('',#2840,#2841,#1639,.T.);
#3578=EDGE_CURVE('',#2841,#2842,#1640,.T.);
#3579=EDGE_CURVE('',#2842,#2843,#1641,.T.);
#3580=EDGE_CURVE('',#2843,#2844,#1642,.T.);
#3581=EDGE_CURVE('',#2844,#2845,#1643,.T.);
#3582=EDGE_CURVE('',#2845,#2840,#1644,.T.);
#3583=EDGE_CURVE('',#2846,#2829,#1645,.T.);
#3584=EDGE_CURVE('',#2829,#2847,#1646,.T.);
#3585=EDGE_CURVE('',#2847,#2842,#1647,.T.);
#3586=EDGE_CURVE('',#2846,#2841,#1648,.T.);
#3587=EDGE_CURVE('',#2847,#2828,#1649,.T.);
#3588=EDGE_CURVE('',#2828,#2848,#1650,.T.);
#3589=EDGE_CURVE('',#2848,#2843,#1651,.T.);
#3590=EDGE_CURVE('',#2848,#2827,#1652,.T.);
#3591=EDGE_CURVE('',#2827,#2849,#1653,.T.);
#3592=EDGE_CURVE('',#2849,#2844,#1654,.T.);
#3593=EDGE_CURVE('',#2849,#2832,#1655,.T.);
#3594=EDGE_CURVE('',#2832,#2850,#1656,.T.);
#3595=EDGE_CURVE('',#2850,#2845,#1657,.T.);
#3596=EDGE_CURVE('',#2850,#2831,#1658,.T.);
#3597=EDGE_CURVE('',#2831,#2851,#1659,.T.);
#3598=EDGE_CURVE('',#2851,#2840,#1660,.T.);
#3599=EDGE_CURVE('',#2851,#2830,#1661,.T.);
#3600=EDGE_CURVE('',#2830,#2846,#1662,.T.);
#3601=EDGE_CURVE('',#2852,#2853,#1663,.T.);
#3602=EDGE_CURVE('',#2853,#2854,#2362,.T.);
#3603=EDGE_CURVE('',#2854,#2855,#2363,.T.);
#3604=EDGE_CURVE('',#2855,#2856,#2364,.T.);
#3605=EDGE_CURVE('',#2856,#2857,#2365,.T.);
#3606=EDGE_CURVE('',#2857,#2858,#2366,.T.);
#3607=EDGE_CURVE('',#2858,#2853,#2367,.T.);
#3608=EDGE_CURVE('',#2859,#2859,#2368,.T.);
#3609=EDGE_CURVE('',#2859,#2860,#2369,.T.);
#3610=EDGE_CURVE('',#2860,#2860,#2370,.T.);
#3611=EDGE_CURVE('',#2861,#2861,#2371,.T.);
#3612=EDGE_CURVE('',#2861,#2862,#1664,.T.);
#3613=EDGE_CURVE('',#2862,#2862,#2372,.T.);
#3614=EDGE_CURVE('',#2860,#2861,#1665,.T.);
#3615=EDGE_CURVE('',#2863,#2863,#2373,.T.);
#3616=EDGE_CURVE('',#2863,#2864,#1666,.T.);
#3617=EDGE_CURVE('',#2864,#2864,#2374,.T.);
#3618=EDGE_CURVE('',#2865,#2865,#2375,.T.);
#3619=EDGE_CURVE('',#2866,#2867,#1667,.T.);
#3620=EDGE_CURVE('',#2867,#2868,#1668,.T.);
#3621=EDGE_CURVE('',#2868,#2869,#1669,.T.);
#3622=EDGE_CURVE('',#2869,#2870,#1670,.T.);
#3623=EDGE_CURVE('',#2870,#2871,#1671,.T.);
#3624=EDGE_CURVE('',#2871,#2866,#1672,.T.);
#3625=EDGE_CURVE('',#2872,#2855,#1673,.T.);
#3626=EDGE_CURVE('',#2855,#2873,#1674,.T.);
#3627=EDGE_CURVE('',#2873,#2868,#1675,.T.);
#3628=EDGE_CURVE('',#2872,#2867,#1676,.T.);
#3629=EDGE_CURVE('',#2873,#2854,#1677,.T.);
#3630=EDGE_CURVE('',#2854,#2874,#1678,.T.);
#3631=EDGE_CURVE('',#2874,#2869,#1679,.T.);
#3632=EDGE_CURVE('',#2874,#2853,#1680,.T.);
#3633=EDGE_CURVE('',#2853,#2875,#1681,.T.);
#3634=EDGE_CURVE('',#2875,#2870,#1682,.T.);
#3635=EDGE_CURVE('',#2875,#2858,#1683,.T.);
#3636=EDGE_CURVE('',#2858,#2876,#1684,.T.);
#3637=EDGE_CURVE('',#2876,#2871,#1685,.T.);
#3638=EDGE_CURVE('',#2876,#2857,#1686,.T.);
#3639=EDGE_CURVE('',#2857,#2877,#1687,.T.);
#3640=EDGE_CURVE('',#2877,#2866,#1688,.T.);
#3641=EDGE_CURVE('',#2877,#2856,#1689,.T.);
#3642=EDGE_CURVE('',#2856,#2872,#1690,.T.);
#3643=ORIENTED_EDGE('',*,*,#2878,.T.);
#3644=ORIENTED_EDGE('',*,*,#2879,.T.);
#3645=ORIENTED_EDGE('',*,*,#2880,.F.);
#3646=ORIENTED_EDGE('',*,*,#2879,.F.);
#3647=ORIENTED_EDGE('',*,*,#2881,.T.);
#3648=ORIENTED_EDGE('',*,*,#2882,.T.);
#3649=ORIENTED_EDGE('',*,*,#2883,.F.);
#3650=ORIENTED_EDGE('',*,*,#2882,.F.);
#3651=ORIENTED_EDGE('',*,*,#2884,.T.);
#3652=ORIENTED_EDGE('',*,*,#2885,.T.);
#3653=ORIENTED_EDGE('',*,*,#2886,.F.);
#3654=ORIENTED_EDGE('',*,*,#2885,.F.);
#3655=ORIENTED_EDGE('',*,*,#2887,.T.);
#3656=ORIENTED_EDGE('',*,*,#2888,.T.);
#3657=ORIENTED_EDGE('',*,*,#2889,.F.);
#3658=ORIENTED_EDGE('',*,*,#2888,.F.);
#3659=ORIENTED_EDGE('',*,*,#2890,.T.);
#3660=ORIENTED_EDGE('',*,*,#2891,.T.);
#3661=ORIENTED_EDGE('',*,*,#2892,.F.);
#3662=ORIENTED_EDGE('',*,*,#2891,.F.);
#3663=ORIENTED_EDGE('',*,*,#2893,.T.);
#3664=ORIENTED_EDGE('',*,*,#2894,.T.);
#3665=ORIENTED_EDGE('',*,*,#2895,.F.);
#3666=ORIENTED_EDGE('',*,*,#2894,.F.);
#3667=ORIENTED_EDGE('',*,*,#2896,.T.);
#3668=ORIENTED_EDGE('',*,*,#2897,.T.);
#3669=ORIENTED_EDGE('',*,*,#2898,.F.);
#3670=ORIENTED_EDGE('',*,*,#2897,.F.);
#3671=ORIENTED_EDGE('',*,*,#2899,.F.);
#3672=ORIENTED_EDGE('',*,*,#2900,.T.);
#3673=ORIENTED_EDGE('',*,*,#2901,.T.);
#3674=ORIENTED_EDGE('',*,*,#2902,.F.);
#3675=ORIENTED_EDGE('',*,*,#2902,.T.);
#3676=ORIENTED_EDGE('',*,*,#2903,.T.);
#3677=ORIENTED_EDGE('',*,*,#2904,.F.);
#3678=ORIENTED_EDGE('',*,*,#2905,.F.);
#3679=ORIENTED_EDGE('',*,*,#2904,.T.);
#3680=ORIENTED_EDGE('',*,*,#2906,.T.);
#3681=ORIENTED_EDGE('',*,*,#2907,.F.);
#3682=ORIENTED_EDGE('',*,*,#2908,.F.);
#3683=ORIENTED_EDGE('',*,*,#2907,.T.);
#3684=ORIENTED_EDGE('',*,*,#2909,.T.);
#3685=ORIENTED_EDGE('',*,*,#2910,.F.);
#3686=ORIENTED_EDGE('',*,*,#2911,.F.);
#3687=ORIENTED_EDGE('',*,*,#2910,.T.);
#3688=ORIENTED_EDGE('',*,*,#2912,.T.);
#3689=ORIENTED_EDGE('',*,*,#2913,.F.);
#3690=ORIENTED_EDGE('',*,*,#2914,.F.);
#3691=ORIENTED_EDGE('',*,*,#2913,.T.);
#3692=ORIENTED_EDGE('',*,*,#2915,.T.);
#3693=ORIENTED_EDGE('',*,*,#2916,.F.);
#3694=ORIENTED_EDGE('',*,*,#2917,.F.);
#3695=ORIENTED_EDGE('',*,*,#2916,.T.);
#3696=ORIENTED_EDGE('',*,*,#2918,.T.);
#3697=ORIENTED_EDGE('',*,*,#2919,.F.);
#3698=ORIENTED_EDGE('',*,*,#2920,.F.);
#3699=ORIENTED_EDGE('',*,*,#2919,.T.);
#3700=ORIENTED_EDGE('',*,*,#2921,.F.);
#3701=ORIENTED_EDGE('',*,*,#2900,.F.);
#3702=ORIENTED_EDGE('',*,*,#2922,.F.);
#3703=ORIENTED_EDGE('',*,*,#2899,.T.);
#3704=ORIENTED_EDGE('',*,*,#2905,.T.);
#3705=ORIENTED_EDGE('',*,*,#2908,.T.);
#3706=ORIENTED_EDGE('',*,*,#2911,.T.);
#3707=ORIENTED_EDGE('',*,*,#2914,.T.);
#3708=ORIENTED_EDGE('',*,*,#2917,.T.);
#3709=ORIENTED_EDGE('',*,*,#2920,.T.);
#3710=ORIENTED_EDGE('',*,*,#2922,.T.);
#3711=ORIENTED_EDGE('',*,*,#2896,.F.);
#3712=ORIENTED_EDGE('',*,*,#2890,.F.);
#3713=ORIENTED_EDGE('',*,*,#2884,.F.);
#3714=ORIENTED_EDGE('',*,*,#2878,.F.);
#3715=ORIENTED_EDGE('',*,*,#2881,.F.);
#3716=ORIENTED_EDGE('',*,*,#2887,.F.);
#3717=ORIENTED_EDGE('',*,*,#2893,.F.);
#3718=ORIENTED_EDGE('',*,*,#2921,.T.);
#3719=ORIENTED_EDGE('',*,*,#2918,.F.);
#3720=ORIENTED_EDGE('',*,*,#2915,.F.);
#3721=ORIENTED_EDGE('',*,*,#2912,.F.);
#3722=ORIENTED_EDGE('',*,*,#2909,.F.);
#3723=ORIENTED_EDGE('',*,*,#2906,.F.);
#3724=ORIENTED_EDGE('',*,*,#2903,.F.);
#3725=ORIENTED_EDGE('',*,*,#2901,.F.);
#3726=ORIENTED_EDGE('',*,*,#2898,.T.);
#3727=ORIENTED_EDGE('',*,*,#2895,.T.);
#3728=ORIENTED_EDGE('',*,*,#2892,.T.);
#3729=ORIENTED_EDGE('',*,*,#2889,.T.);
#3730=ORIENTED_EDGE('',*,*,#2886,.T.);
#3731=ORIENTED_EDGE('',*,*,#2883,.T.);
#3732=ORIENTED_EDGE('',*,*,#2880,.T.);
#3733=ORIENTED_EDGE('',*,*,#2923,.F.);
#3734=ORIENTED_EDGE('',*,*,#2924,.T.);
#3735=ORIENTED_EDGE('',*,*,#2925,.F.);
#3736=ORIENTED_EDGE('',*,*,#2924,.F.);
#3737=ORIENTED_EDGE('',*,*,#2926,.F.);
#3738=ORIENTED_EDGE('',*,*,#2927,.T.);
#3739=ORIENTED_EDGE('',*,*,#2928,.F.);
#3740=ORIENTED_EDGE('',*,*,#2927,.F.);
#3741=ORIENTED_EDGE('',*,*,#2929,.F.);
#3742=ORIENTED_EDGE('',*,*,#2930,.T.);
#3743=ORIENTED_EDGE('',*,*,#2931,.F.);
#3744=ORIENTED_EDGE('',*,*,#2930,.F.);
#3745=ORIENTED_EDGE('',*,*,#2932,.F.);
#3746=ORIENTED_EDGE('',*,*,#2933,.T.);
#3747=ORIENTED_EDGE('',*,*,#2934,.F.);
#3748=ORIENTED_EDGE('',*,*,#2933,.F.);
#3749=ORIENTED_EDGE('',*,*,#2935,.T.);
#3750=ORIENTED_EDGE('',*,*,#2936,.T.);
#3751=ORIENTED_EDGE('',*,*,#2937,.T.);
#3752=ORIENTED_EDGE('',*,*,#2938,.F.);
#3753=ORIENTED_EDGE('',*,*,#2939,.F.);
#3754=ORIENTED_EDGE('',*,*,#2940,.T.);
#3755=ORIENTED_EDGE('',*,*,#2941,.F.);
#3756=ORIENTED_EDGE('',*,*,#2940,.F.);
#3757=ORIENTED_EDGE('',*,*,#2942,.F.);
#3758=ORIENTED_EDGE('',*,*,#2943,.T.);
#3759=ORIENTED_EDGE('',*,*,#2944,.F.);
#3760=ORIENTED_EDGE('',*,*,#2943,.F.);
#3761=ORIENTED_EDGE('',*,*,#2945,.F.);
#3762=ORIENTED_EDGE('',*,*,#2946,.T.);
#3763=ORIENTED_EDGE('',*,*,#2947,.F.);
#3764=ORIENTED_EDGE('',*,*,#2946,.F.);
#3765=ORIENTED_EDGE('',*,*,#2936,.F.);
#3766=ORIENTED_EDGE('',*,*,#2948,.T.);
#3767=ORIENTED_EDGE('',*,*,#2949,.T.);
#3768=ORIENTED_EDGE('',*,*,#2950,.T.);
#3769=ORIENTED_EDGE('',*,*,#2949,.F.);
#3770=ORIENTED_EDGE('',*,*,#2951,.T.);
#3771=ORIENTED_EDGE('',*,*,#2952,.T.);
#3772=ORIENTED_EDGE('',*,*,#2953,.T.);
#3773=ORIENTED_EDGE('',*,*,#2952,.F.);
#3774=ORIENTED_EDGE('',*,*,#2954,.T.);
#3775=ORIENTED_EDGE('',*,*,#2955,.T.);
#3776=ORIENTED_EDGE('',*,*,#2956,.T.);
#3777=ORIENTED_EDGE('',*,*,#2955,.F.);
#3778=ORIENTED_EDGE('',*,*,#2957,.T.);
#3779=ORIENTED_EDGE('',*,*,#2958,.T.);
#3780=ORIENTED_EDGE('',*,*,#2959,.T.);
#3781=ORIENTED_EDGE('',*,*,#2958,.F.);
#3782=ORIENTED_EDGE('',*,*,#2960,.F.);
#3783=ORIENTED_EDGE('',*,*,#2961,.T.);
#3784=ORIENTED_EDGE('',*,*,#2962,.T.);
#3785=ORIENTED_EDGE('',*,*,#2961,.F.);
#3786=ORIENTED_EDGE('',*,*,#2963,.T.);
#3787=ORIENTED_EDGE('',*,*,#2964,.T.);
#3788=ORIENTED_EDGE('',*,*,#2965,.T.);
#3789=ORIENTED_EDGE('',*,*,#2964,.F.);
#3790=ORIENTED_EDGE('',*,*,#2966,.T.);
#3791=ORIENTED_EDGE('',*,*,#2938,.T.);
#3792=ORIENTED_EDGE('',*,*,#2967,.T.);
#3793=ORIENTED_EDGE('',*,*,#2937,.F.);
#3794=ORIENTED_EDGE('',*,*,#2950,.F.);
#3795=ORIENTED_EDGE('',*,*,#2953,.F.);
#3796=ORIENTED_EDGE('',*,*,#2956,.F.);
#3797=ORIENTED_EDGE('',*,*,#2959,.F.);
#3798=ORIENTED_EDGE('',*,*,#2962,.F.);
#3799=ORIENTED_EDGE('',*,*,#2965,.F.);
#3800=ORIENTED_EDGE('',*,*,#2967,.F.);
#3801=ORIENTED_EDGE('',*,*,#2941,.T.);
#3802=ORIENTED_EDGE('',*,*,#2944,.T.);
#3803=ORIENTED_EDGE('',*,*,#2947,.T.);
#3804=ORIENTED_EDGE('',*,*,#2925,.T.);
#3805=ORIENTED_EDGE('',*,*,#2928,.T.);
#3806=ORIENTED_EDGE('',*,*,#2931,.T.);
#3807=ORIENTED_EDGE('',*,*,#2934,.T.);
#3808=ORIENTED_EDGE('',*,*,#2966,.F.);
#3809=ORIENTED_EDGE('',*,*,#2963,.F.);
#3810=ORIENTED_EDGE('',*,*,#2960,.T.);
#3811=ORIENTED_EDGE('',*,*,#2957,.F.);
#3812=ORIENTED_EDGE('',*,*,#2954,.F.);
#3813=ORIENTED_EDGE('',*,*,#2951,.F.);
#3814=ORIENTED_EDGE('',*,*,#2948,.F.);
#3815=ORIENTED_EDGE('',*,*,#2935,.F.);
#3816=ORIENTED_EDGE('',*,*,#2939,.T.);
#3817=ORIENTED_EDGE('',*,*,#2932,.T.);
#3818=ORIENTED_EDGE('',*,*,#2942,.T.);
#3819=ORIENTED_EDGE('',*,*,#2929,.T.);
#3820=ORIENTED_EDGE('',*,*,#2945,.T.);
#3821=ORIENTED_EDGE('',*,*,#2926,.T.);
#3822=ORIENTED_EDGE('',*,*,#2923,.T.);
#3823=ORIENTED_EDGE('',*,*,#2968,.T.);
#3824=ORIENTED_EDGE('',*,*,#2969,.F.);
#3825=ORIENTED_EDGE('',*,*,#2970,.F.);
#3826=ORIENTED_EDGE('',*,*,#2971,.T.);
#3827=ORIENTED_EDGE('',*,*,#2972,.T.);
#3828=ORIENTED_EDGE('',*,*,#2973,.F.);
#3829=ORIENTED_EDGE('',*,*,#2974,.F.);
#3830=ORIENTED_EDGE('',*,*,#2969,.T.);
#3831=ORIENTED_EDGE('',*,*,#2975,.T.);
#3832=ORIENTED_EDGE('',*,*,#2976,.F.);
#3833=ORIENTED_EDGE('',*,*,#2977,.F.);
#3834=ORIENTED_EDGE('',*,*,#2973,.T.);
#3835=ORIENTED_EDGE('',*,*,#2978,.T.);
#3836=ORIENTED_EDGE('',*,*,#2979,.F.);
#3837=ORIENTED_EDGE('',*,*,#2980,.F.);
#3838=ORIENTED_EDGE('',*,*,#2976,.T.);
#3839=ORIENTED_EDGE('',*,*,#2981,.T.);
#3840=ORIENTED_EDGE('',*,*,#2982,.F.);
#3841=ORIENTED_EDGE('',*,*,#2983,.F.);
#3842=ORIENTED_EDGE('',*,*,#2979,.T.);
#3843=ORIENTED_EDGE('',*,*,#2984,.T.);
#3844=ORIENTED_EDGE('',*,*,#2971,.F.);
#3845=ORIENTED_EDGE('',*,*,#2985,.F.);
#3846=ORIENTED_EDGE('',*,*,#2982,.T.);
#3847=ORIENTED_EDGE('',*,*,#2970,.T.);
#3848=ORIENTED_EDGE('',*,*,#2974,.T.);
#3849=ORIENTED_EDGE('',*,*,#2977,.T.);
#3850=ORIENTED_EDGE('',*,*,#2980,.T.);
#3851=ORIENTED_EDGE('',*,*,#2983,.T.);
#3852=ORIENTED_EDGE('',*,*,#2985,.T.);
#3853=ORIENTED_EDGE('',*,*,#2968,.F.);
#3854=ORIENTED_EDGE('',*,*,#2984,.F.);
#3855=ORIENTED_EDGE('',*,*,#2981,.F.);
#3856=ORIENTED_EDGE('',*,*,#2978,.F.);
#3857=ORIENTED_EDGE('',*,*,#2975,.F.);
#3858=ORIENTED_EDGE('',*,*,#2972,.F.);
#3859=ORIENTED_EDGE('',*,*,#2986,.T.);
#3860=ORIENTED_EDGE('',*,*,#2987,.F.);
#3861=ORIENTED_EDGE('',*,*,#2988,.F.);
#3862=ORIENTED_EDGE('',*,*,#2989,.T.);
#3863=ORIENTED_EDGE('',*,*,#2990,.T.);
#3864=ORIENTED_EDGE('',*,*,#2991,.F.);
#3865=ORIENTED_EDGE('',*,*,#2992,.F.);
#3866=ORIENTED_EDGE('',*,*,#2987,.T.);
#3867=ORIENTED_EDGE('',*,*,#2993,.T.);
#3868=ORIENTED_EDGE('',*,*,#2994,.F.);
#3869=ORIENTED_EDGE('',*,*,#2995,.F.);
#3870=ORIENTED_EDGE('',*,*,#2991,.T.);
#3871=ORIENTED_EDGE('',*,*,#2996,.T.);
#3872=ORIENTED_EDGE('',*,*,#2997,.F.);
#3873=ORIENTED_EDGE('',*,*,#2998,.F.);
#3874=ORIENTED_EDGE('',*,*,#2994,.T.);
#3875=ORIENTED_EDGE('',*,*,#2999,.T.);
#3876=ORIENTED_EDGE('',*,*,#3000,.F.);
#3877=ORIENTED_EDGE('',*,*,#3001,.F.);
#3878=ORIENTED_EDGE('',*,*,#2997,.T.);
#3879=ORIENTED_EDGE('',*,*,#3002,.T.);
#3880=ORIENTED_EDGE('',*,*,#2989,.F.);
#3881=ORIENTED_EDGE('',*,*,#3003,.F.);
#3882=ORIENTED_EDGE('',*,*,#3000,.T.);
#3883=ORIENTED_EDGE('',*,*,#2988,.T.);
#3884=ORIENTED_EDGE('',*,*,#2992,.T.);
#3885=ORIENTED_EDGE('',*,*,#2995,.T.);
#3886=ORIENTED_EDGE('',*,*,#2998,.T.);
#3887=ORIENTED_EDGE('',*,*,#3001,.T.);
#3888=ORIENTED_EDGE('',*,*,#3003,.T.);
#3889=ORIENTED_EDGE('',*,*,#2986,.F.);
#3890=ORIENTED_EDGE('',*,*,#3002,.F.);
#3891=ORIENTED_EDGE('',*,*,#2999,.F.);
#3892=ORIENTED_EDGE('',*,*,#2996,.F.);
#3893=ORIENTED_EDGE('',*,*,#2993,.F.);
#3894=ORIENTED_EDGE('',*,*,#2990,.F.);
#3895=ORIENTED_EDGE('',*,*,#3004,.T.);
#3896=ORIENTED_EDGE('',*,*,#3005,.F.);
#3897=ORIENTED_EDGE('',*,*,#3006,.F.);
#3898=ORIENTED_EDGE('',*,*,#3007,.T.);
#3899=ORIENTED_EDGE('',*,*,#3008,.T.);
#3900=ORIENTED_EDGE('',*,*,#3009,.F.);
#3901=ORIENTED_EDGE('',*,*,#3010,.F.);
#3902=ORIENTED_EDGE('',*,*,#3005,.T.);
#3903=ORIENTED_EDGE('',*,*,#3011,.T.);
#3904=ORIENTED_EDGE('',*,*,#3012,.F.);
#3905=ORIENTED_EDGE('',*,*,#3013,.F.);
#3906=ORIENTED_EDGE('',*,*,#3009,.T.);
#3907=ORIENTED_EDGE('',*,*,#3014,.T.);
#3908=ORIENTED_EDGE('',*,*,#3015,.F.);
#3909=ORIENTED_EDGE('',*,*,#3016,.F.);
#3910=ORIENTED_EDGE('',*,*,#3012,.T.);
#3911=ORIENTED_EDGE('',*,*,#3017,.T.);
#3912=ORIENTED_EDGE('',*,*,#3018,.F.);
#3913=ORIENTED_EDGE('',*,*,#3019,.F.);
#3914=ORIENTED_EDGE('',*,*,#3015,.T.);
#3915=ORIENTED_EDGE('',*,*,#3020,.T.);
#3916=ORIENTED_EDGE('',*,*,#3007,.F.);
#3917=ORIENTED_EDGE('',*,*,#3021,.F.);
#3918=ORIENTED_EDGE('',*,*,#3018,.T.);
#3919=ORIENTED_EDGE('',*,*,#3006,.T.);
#3920=ORIENTED_EDGE('',*,*,#3010,.T.);
#3921=ORIENTED_EDGE('',*,*,#3013,.T.);
#3922=ORIENTED_EDGE('',*,*,#3016,.T.);
#3923=ORIENTED_EDGE('',*,*,#3019,.T.);
#3924=ORIENTED_EDGE('',*,*,#3021,.T.);
#3925=ORIENTED_EDGE('',*,*,#3004,.F.);
#3926=ORIENTED_EDGE('',*,*,#3020,.F.);
#3927=ORIENTED_EDGE('',*,*,#3017,.F.);
#3928=ORIENTED_EDGE('',*,*,#3014,.F.);
#3929=ORIENTED_EDGE('',*,*,#3011,.F.);
#3930=ORIENTED_EDGE('',*,*,#3008,.F.);
#3931=ORIENTED_EDGE('',*,*,#3022,.F.);
#3932=ORIENTED_EDGE('',*,*,#3023,.T.);
#3933=ORIENTED_EDGE('',*,*,#3024,.T.);
#3934=ORIENTED_EDGE('',*,*,#3023,.F.);
#3935=ORIENTED_EDGE('',*,*,#3025,.F.);
#3936=ORIENTED_EDGE('',*,*,#3026,.T.);
#3937=ORIENTED_EDGE('',*,*,#3027,.T.);
#3938=ORIENTED_EDGE('',*,*,#3028,.F.);
#3939=ORIENTED_EDGE('',*,*,#3029,.F.);
#3940=ORIENTED_EDGE('',*,*,#3030,.T.);
#3941=ORIENTED_EDGE('',*,*,#3031,.T.);
#3942=ORIENTED_EDGE('',*,*,#3030,.F.);
#3943=ORIENTED_EDGE('',*,*,#3032,.T.);
#3944=ORIENTED_EDGE('',*,*,#3033,.T.);
#3945=ORIENTED_EDGE('',*,*,#3034,.F.);
#3946=ORIENTED_EDGE('',*,*,#3033,.F.);
#3947=ORIENTED_EDGE('',*,*,#3035,.T.);
#3948=ORIENTED_EDGE('',*,*,#3036,.T.);
#3949=ORIENTED_EDGE('',*,*,#3037,.F.);
#3950=ORIENTED_EDGE('',*,*,#3036,.F.);
#3951=ORIENTED_EDGE('',*,*,#3022,.T.);
#3952=ORIENTED_EDGE('',*,*,#3034,.T.);
#3953=ORIENTED_EDGE('',*,*,#3029,.T.);
#3954=ORIENTED_EDGE('',*,*,#3032,.F.);
#3955=ORIENTED_EDGE('',*,*,#3038,.T.);
#3956=ORIENTED_EDGE('',*,*,#3039,.T.);
#3957=ORIENTED_EDGE('',*,*,#3040,.T.);
#3958=ORIENTED_EDGE('',*,*,#3041,.T.);
#3959=ORIENTED_EDGE('',*,*,#3042,.T.);
#3960=ORIENTED_EDGE('',*,*,#3043,.T.);
#3961=ORIENTED_EDGE('',*,*,#3044,.T.);
#3962=ORIENTED_EDGE('',*,*,#3045,.T.);
#3963=ORIENTED_EDGE('',*,*,#3046,.T.);
#3964=ORIENTED_EDGE('',*,*,#3047,.T.);
#3965=ORIENTED_EDGE('',*,*,#3048,.T.);
#3966=ORIENTED_EDGE('',*,*,#3049,.T.);
#3967=ORIENTED_EDGE('',*,*,#3050,.T.);
#3968=ORIENTED_EDGE('',*,*,#3051,.T.);
#3969=ORIENTED_EDGE('',*,*,#3052,.T.);
#3970=ORIENTED_EDGE('',*,*,#3053,.T.);
#3971=ORIENTED_EDGE('',*,*,#3054,.T.);
#3972=ORIENTED_EDGE('',*,*,#3055,.T.);
#3973=ORIENTED_EDGE('',*,*,#3056,.T.);
#3974=ORIENTED_EDGE('',*,*,#3057,.T.);
#3975=ORIENTED_EDGE('',*,*,#3058,.F.);
#3976=ORIENTED_EDGE('',*,*,#3059,.F.);
#3977=ORIENTED_EDGE('',*,*,#3060,.F.);
#3978=ORIENTED_EDGE('',*,*,#3061,.F.);
#3979=ORIENTED_EDGE('',*,*,#3062,.F.);
#3980=ORIENTED_EDGE('',*,*,#3063,.F.);
#3981=ORIENTED_EDGE('',*,*,#3064,.F.);
#3982=ORIENTED_EDGE('',*,*,#3065,.F.);
#3983=ORIENTED_EDGE('',*,*,#3066,.F.);
#3984=ORIENTED_EDGE('',*,*,#3067,.F.);
#3985=ORIENTED_EDGE('',*,*,#3068,.F.);
#3986=ORIENTED_EDGE('',*,*,#3069,.F.);
#3987=ORIENTED_EDGE('',*,*,#3070,.F.);
#3988=ORIENTED_EDGE('',*,*,#3071,.F.);
#3989=ORIENTED_EDGE('',*,*,#3072,.F.);
#3990=ORIENTED_EDGE('',*,*,#3073,.F.);
#3991=ORIENTED_EDGE('',*,*,#3074,.F.);
#3992=ORIENTED_EDGE('',*,*,#3075,.F.);
#3993=ORIENTED_EDGE('',*,*,#3035,.F.);
#3994=ORIENTED_EDGE('',*,*,#3076,.F.);
#3995=ORIENTED_EDGE('',*,*,#3077,.F.);
#3996=ORIENTED_EDGE('',*,*,#3078,.F.);
#3997=ORIENTED_EDGE('',*,*,#3079,.F.);
#3998=ORIENTED_EDGE('',*,*,#3080,.F.);
#3999=ORIENTED_EDGE('',*,*,#3081,.F.);
#4000=ORIENTED_EDGE('',*,*,#3082,.F.);
#4001=ORIENTED_EDGE('',*,*,#3083,.F.);
#4002=ORIENTED_EDGE('',*,*,#3084,.F.);
#4003=ORIENTED_EDGE('',*,*,#3085,.F.);
#4004=ORIENTED_EDGE('',*,*,#3086,.F.);
#4005=ORIENTED_EDGE('',*,*,#3087,.F.);
#4006=ORIENTED_EDGE('',*,*,#3088,.F.);
#4007=ORIENTED_EDGE('',*,*,#3089,.F.);
#4008=ORIENTED_EDGE('',*,*,#3090,.F.);
#4009=ORIENTED_EDGE('',*,*,#3091,.F.);
#4010=ORIENTED_EDGE('',*,*,#3092,.F.);
#4011=ORIENTED_EDGE('',*,*,#3093,.F.);
#4012=ORIENTED_EDGE('',*,*,#3094,.F.);
#4013=ORIENTED_EDGE('',*,*,#3095,.F.);
#4014=ORIENTED_EDGE('',*,*,#3096,.F.);
#4015=ORIENTED_EDGE('',*,*,#3097,.F.);
#4016=ORIENTED_EDGE('',*,*,#3098,.F.);
#4017=ORIENTED_EDGE('',*,*,#3099,.F.);
#4018=ORIENTED_EDGE('',*,*,#3100,.F.);
#4019=ORIENTED_EDGE('',*,*,#3101,.F.);
#4020=ORIENTED_EDGE('',*,*,#3102,.F.);
#4021=ORIENTED_EDGE('',*,*,#3103,.F.);
#4022=ORIENTED_EDGE('',*,*,#3104,.F.);
#4023=ORIENTED_EDGE('',*,*,#3105,.F.);
#4024=ORIENTED_EDGE('',*,*,#3027,.F.);
#4025=ORIENTED_EDGE('',*,*,#3106,.F.);
#4026=ORIENTED_EDGE('',*,*,#3107,.F.);
#4027=ORIENTED_EDGE('',*,*,#3108,.F.);
#4028=ORIENTED_EDGE('',*,*,#3109,.F.);
#4029=ORIENTED_EDGE('',*,*,#3110,.F.);
#4030=ORIENTED_EDGE('',*,*,#3111,.F.);
#4031=ORIENTED_EDGE('',*,*,#3112,.F.);
#4032=ORIENTED_EDGE('',*,*,#3037,.T.);
#4033=ORIENTED_EDGE('',*,*,#3076,.T.);
#4034=ORIENTED_EDGE('',*,*,#3113,.F.);
#4035=ORIENTED_EDGE('',*,*,#3038,.F.);
#4036=ORIENTED_EDGE('',*,*,#3114,.T.);
#4037=ORIENTED_EDGE('',*,*,#3095,.T.);
#4038=ORIENTED_EDGE('',*,*,#3115,.F.);
#4039=ORIENTED_EDGE('',*,*,#3039,.F.);
#4040=ORIENTED_EDGE('',*,*,#3113,.T.);
#4041=ORIENTED_EDGE('',*,*,#3094,.T.);
#4042=ORIENTED_EDGE('',*,*,#3116,.F.);
#4043=ORIENTED_EDGE('',*,*,#3040,.F.);
#4044=ORIENTED_EDGE('',*,*,#3115,.T.);
#4045=ORIENTED_EDGE('',*,*,#3093,.T.);
#4046=ORIENTED_EDGE('',*,*,#3117,.F.);
#4047=ORIENTED_EDGE('',*,*,#3041,.F.);
#4048=ORIENTED_EDGE('',*,*,#3116,.T.);
#4049=ORIENTED_EDGE('',*,*,#3092,.T.);
#4050=ORIENTED_EDGE('',*,*,#3118,.F.);
#4051=ORIENTED_EDGE('',*,*,#3042,.F.);
#4052=ORIENTED_EDGE('',*,*,#3117,.T.);
#4053=ORIENTED_EDGE('',*,*,#3091,.T.);
#4054=ORIENTED_EDGE('',*,*,#3119,.F.);
#4055=ORIENTED_EDGE('',*,*,#3043,.F.);
#4056=ORIENTED_EDGE('',*,*,#3118,.T.);
#4057=ORIENTED_EDGE('',*,*,#3090,.T.);
#4058=ORIENTED_EDGE('',*,*,#3120,.F.);
#4059=ORIENTED_EDGE('',*,*,#3044,.F.);
#4060=ORIENTED_EDGE('',*,*,#3119,.T.);
#4061=ORIENTED_EDGE('',*,*,#3089,.T.);
#4062=ORIENTED_EDGE('',*,*,#3121,.F.);
#4063=ORIENTED_EDGE('',*,*,#3045,.F.);
#4064=ORIENTED_EDGE('',*,*,#3120,.T.);
#4065=ORIENTED_EDGE('',*,*,#3088,.T.);
#4066=ORIENTED_EDGE('',*,*,#3122,.F.);
#4067=ORIENTED_EDGE('',*,*,#3046,.F.);
#4068=ORIENTED_EDGE('',*,*,#3121,.T.);
#4069=ORIENTED_EDGE('',*,*,#3087,.T.);
#4070=ORIENTED_EDGE('',*,*,#3123,.F.);
#4071=ORIENTED_EDGE('',*,*,#3047,.F.);
#4072=ORIENTED_EDGE('',*,*,#3122,.T.);
#4073=ORIENTED_EDGE('',*,*,#3086,.T.);
#4074=ORIENTED_EDGE('',*,*,#3124,.F.);
#4075=ORIENTED_EDGE('',*,*,#3048,.F.);
#4076=ORIENTED_EDGE('',*,*,#3123,.T.);
#4077=ORIENTED_EDGE('',*,*,#3085,.T.);
#4078=ORIENTED_EDGE('',*,*,#3125,.F.);
#4079=ORIENTED_EDGE('',*,*,#3049,.F.);
#4080=ORIENTED_EDGE('',*,*,#3124,.T.);
#4081=ORIENTED_EDGE('',*,*,#3084,.T.);
#4082=ORIENTED_EDGE('',*,*,#3126,.F.);
#4083=ORIENTED_EDGE('',*,*,#3050,.F.);
#4084=ORIENTED_EDGE('',*,*,#3125,.T.);
#4085=ORIENTED_EDGE('',*,*,#3083,.T.);
#4086=ORIENTED_EDGE('',*,*,#3127,.F.);
#4087=ORIENTED_EDGE('',*,*,#3051,.F.);
#4088=ORIENTED_EDGE('',*,*,#3126,.T.);
#4089=ORIENTED_EDGE('',*,*,#3082,.T.);
#4090=ORIENTED_EDGE('',*,*,#3128,.F.);
#4091=ORIENTED_EDGE('',*,*,#3052,.F.);
#4092=ORIENTED_EDGE('',*,*,#3127,.T.);
#4093=ORIENTED_EDGE('',*,*,#3081,.T.);
#4094=ORIENTED_EDGE('',*,*,#3129,.F.);
#4095=ORIENTED_EDGE('',*,*,#3053,.F.);
#4096=ORIENTED_EDGE('',*,*,#3128,.T.);
#4097=ORIENTED_EDGE('',*,*,#3080,.T.);
#4098=ORIENTED_EDGE('',*,*,#3130,.F.);
#4099=ORIENTED_EDGE('',*,*,#3054,.F.);
#4100=ORIENTED_EDGE('',*,*,#3129,.T.);
#4101=ORIENTED_EDGE('',*,*,#3079,.T.);
#4102=ORIENTED_EDGE('',*,*,#3131,.F.);
#4103=ORIENTED_EDGE('',*,*,#3055,.F.);
#4104=ORIENTED_EDGE('',*,*,#3130,.T.);
#4105=ORIENTED_EDGE('',*,*,#3078,.T.);
#4106=ORIENTED_EDGE('',*,*,#3132,.F.);
#4107=ORIENTED_EDGE('',*,*,#3056,.F.);
#4108=ORIENTED_EDGE('',*,*,#3131,.T.);
#4109=ORIENTED_EDGE('',*,*,#3077,.T.);
#4110=ORIENTED_EDGE('',*,*,#3114,.F.);
#4111=ORIENTED_EDGE('',*,*,#3057,.F.);
#4112=ORIENTED_EDGE('',*,*,#3132,.T.);
#4113=ORIENTED_EDGE('',*,*,#3071,.T.);
#4114=ORIENTED_EDGE('',*,*,#3133,.F.);
#4115=ORIENTED_EDGE('',*,*,#3134,.F.);
#4116=ORIENTED_EDGE('',*,*,#3135,.T.);
#4117=ORIENTED_EDGE('',*,*,#3072,.T.);
#4118=ORIENTED_EDGE('',*,*,#3135,.F.);
#4119=ORIENTED_EDGE('',*,*,#3136,.F.);
#4120=ORIENTED_EDGE('',*,*,#3137,.T.);
#4121=ORIENTED_EDGE('',*,*,#3073,.T.);
#4122=ORIENTED_EDGE('',*,*,#3137,.F.);
#4123=ORIENTED_EDGE('',*,*,#3138,.F.);
#4124=ORIENTED_EDGE('',*,*,#3139,.T.);
#4125=ORIENTED_EDGE('',*,*,#3074,.T.);
#4126=ORIENTED_EDGE('',*,*,#3139,.F.);
#4127=ORIENTED_EDGE('',*,*,#3140,.F.);
#4128=ORIENTED_EDGE('',*,*,#3141,.T.);
#4129=ORIENTED_EDGE('',*,*,#3075,.T.);
#4130=ORIENTED_EDGE('',*,*,#3141,.F.);
#4131=ORIENTED_EDGE('',*,*,#3142,.F.);
#4132=ORIENTED_EDGE('',*,*,#3133,.T.);
#4133=ORIENTED_EDGE('',*,*,#3134,.T.);
#4134=ORIENTED_EDGE('',*,*,#3142,.T.);
#4135=ORIENTED_EDGE('',*,*,#3140,.T.);
#4136=ORIENTED_EDGE('',*,*,#3138,.T.);
#4137=ORIENTED_EDGE('',*,*,#3136,.T.);
#4138=ORIENTED_EDGE('',*,*,#3066,.T.);
#4139=ORIENTED_EDGE('',*,*,#3143,.F.);
#4140=ORIENTED_EDGE('',*,*,#3144,.F.);
#4141=ORIENTED_EDGE('',*,*,#3145,.T.);
#4142=ORIENTED_EDGE('',*,*,#3067,.T.);
#4143=ORIENTED_EDGE('',*,*,#3145,.F.);
#4144=ORIENTED_EDGE('',*,*,#3146,.F.);
#4145=ORIENTED_EDGE('',*,*,#3147,.T.);
#4146=ORIENTED_EDGE('',*,*,#3068,.T.);
#4147=ORIENTED_EDGE('',*,*,#3147,.F.);
#4148=ORIENTED_EDGE('',*,*,#3148,.F.);
#4149=ORIENTED_EDGE('',*,*,#3149,.T.);
#4150=ORIENTED_EDGE('',*,*,#3069,.T.);
#4151=ORIENTED_EDGE('',*,*,#3149,.F.);
#4152=ORIENTED_EDGE('',*,*,#3150,.F.);
#4153=ORIENTED_EDGE('',*,*,#3151,.T.);
#4154=ORIENTED_EDGE('',*,*,#3070,.T.);
#4155=ORIENTED_EDGE('',*,*,#3151,.F.);
#4156=ORIENTED_EDGE('',*,*,#3152,.F.);
#4157=ORIENTED_EDGE('',*,*,#3143,.T.);
#4158=ORIENTED_EDGE('',*,*,#3144,.T.);
#4159=ORIENTED_EDGE('',*,*,#3152,.T.);
#4160=ORIENTED_EDGE('',*,*,#3150,.T.);
#4161=ORIENTED_EDGE('',*,*,#3148,.T.);
#4162=ORIENTED_EDGE('',*,*,#3146,.T.);
#4163=ORIENTED_EDGE('',*,*,#3058,.T.);
#4164=ORIENTED_EDGE('',*,*,#3153,.F.);
#4165=ORIENTED_EDGE('',*,*,#3154,.F.);
#4166=ORIENTED_EDGE('',*,*,#3155,.T.);
#4167=ORIENTED_EDGE('',*,*,#3059,.T.);
#4168=ORIENTED_EDGE('',*,*,#3155,.F.);
#4169=ORIENTED_EDGE('',*,*,#3156,.F.);
#4170=ORIENTED_EDGE('',*,*,#3157,.T.);
#4171=ORIENTED_EDGE('',*,*,#3060,.T.);
#4172=ORIENTED_EDGE('',*,*,#3157,.F.);
#4173=ORIENTED_EDGE('',*,*,#3158,.F.);
#4174=ORIENTED_EDGE('',*,*,#3159,.T.);
#4175=ORIENTED_EDGE('',*,*,#3061,.T.);
#4176=ORIENTED_EDGE('',*,*,#3159,.F.);
#4177=ORIENTED_EDGE('',*,*,#3160,.F.);
#4178=ORIENTED_EDGE('',*,*,#3161,.T.);
#4179=ORIENTED_EDGE('',*,*,#3062,.T.);
#4180=ORIENTED_EDGE('',*,*,#3161,.F.);
#4181=ORIENTED_EDGE('',*,*,#3162,.F.);
#4182=ORIENTED_EDGE('',*,*,#3163,.T.);
#4183=ORIENTED_EDGE('',*,*,#3063,.T.);
#4184=ORIENTED_EDGE('',*,*,#3163,.F.);
#4185=ORIENTED_EDGE('',*,*,#3164,.F.);
#4186=ORIENTED_EDGE('',*,*,#3165,.T.);
#4187=ORIENTED_EDGE('',*,*,#3064,.T.);
#4188=ORIENTED_EDGE('',*,*,#3165,.F.);
#4189=ORIENTED_EDGE('',*,*,#3166,.F.);
#4190=ORIENTED_EDGE('',*,*,#3167,.T.);
#4191=ORIENTED_EDGE('',*,*,#3065,.T.);
#4192=ORIENTED_EDGE('',*,*,#3167,.F.);
#4193=ORIENTED_EDGE('',*,*,#3168,.F.);
#4194=ORIENTED_EDGE('',*,*,#3153,.T.);
#4195=ORIENTED_EDGE('',*,*,#3154,.T.);
#4196=ORIENTED_EDGE('',*,*,#3168,.T.);
#4197=ORIENTED_EDGE('',*,*,#3166,.T.);
#4198=ORIENTED_EDGE('',*,*,#3164,.T.);
#4199=ORIENTED_EDGE('',*,*,#3162,.T.);
#4200=ORIENTED_EDGE('',*,*,#3160,.T.);
#4201=ORIENTED_EDGE('',*,*,#3158,.T.);
#4202=ORIENTED_EDGE('',*,*,#3156,.T.);
#4203=ORIENTED_EDGE('',*,*,#3031,.F.);
#4204=ORIENTED_EDGE('',*,*,#3106,.T.);
#4205=ORIENTED_EDGE('',*,*,#3026,.F.);
#4206=ORIENTED_EDGE('',*,*,#3169,.F.);
#4207=ORIENTED_EDGE('',*,*,#3170,.T.);
#4208=ORIENTED_EDGE('',*,*,#3107,.T.);
#4209=ORIENTED_EDGE('',*,*,#3170,.F.);
#4210=ORIENTED_EDGE('',*,*,#3171,.F.);
#4211=ORIENTED_EDGE('',*,*,#3172,.T.);
#4212=ORIENTED_EDGE('',*,*,#3108,.T.);
#4213=ORIENTED_EDGE('',*,*,#3172,.F.);
#4214=ORIENTED_EDGE('',*,*,#3173,.F.);
#4215=ORIENTED_EDGE('',*,*,#3174,.T.);
#4216=ORIENTED_EDGE('',*,*,#3109,.T.);
#4217=ORIENTED_EDGE('',*,*,#3174,.F.);
#4218=ORIENTED_EDGE('',*,*,#3175,.F.);
#4219=ORIENTED_EDGE('',*,*,#3176,.T.);
#4220=ORIENTED_EDGE('',*,*,#3110,.T.);
#4221=ORIENTED_EDGE('',*,*,#3176,.F.);
#4222=ORIENTED_EDGE('',*,*,#3177,.F.);
#4223=ORIENTED_EDGE('',*,*,#3178,.T.);
#4224=ORIENTED_EDGE('',*,*,#3111,.T.);
#4225=ORIENTED_EDGE('',*,*,#3178,.F.);
#4226=ORIENTED_EDGE('',*,*,#3179,.F.);
#4227=ORIENTED_EDGE('',*,*,#3180,.T.);
#4228=ORIENTED_EDGE('',*,*,#3112,.T.);
#4229=ORIENTED_EDGE('',*,*,#3180,.F.);
#4230=ORIENTED_EDGE('',*,*,#3181,.F.);
#4231=ORIENTED_EDGE('',*,*,#3028,.T.);
#4232=ORIENTED_EDGE('',*,*,#3169,.T.);
#4233=ORIENTED_EDGE('',*,*,#3025,.T.);
#4234=ORIENTED_EDGE('',*,*,#3181,.T.);
#4235=ORIENTED_EDGE('',*,*,#3179,.T.);
#4236=ORIENTED_EDGE('',*,*,#3177,.T.);
#4237=ORIENTED_EDGE('',*,*,#3175,.T.);
#4238=ORIENTED_EDGE('',*,*,#3173,.T.);
#4239=ORIENTED_EDGE('',*,*,#3171,.T.);
#4240=ORIENTED_EDGE('',*,*,#3024,.F.);
#4241=ORIENTED_EDGE('',*,*,#3102,.T.);
#4242=ORIENTED_EDGE('',*,*,#3182,.F.);
#4243=ORIENTED_EDGE('',*,*,#3183,.F.);
#4244=ORIENTED_EDGE('',*,*,#3184,.T.);
#4245=ORIENTED_EDGE('',*,*,#3103,.T.);
#4246=ORIENTED_EDGE('',*,*,#3184,.F.);
#4247=ORIENTED_EDGE('',*,*,#3185,.F.);
#4248=ORIENTED_EDGE('',*,*,#3186,.T.);
#4249=ORIENTED_EDGE('',*,*,#3104,.T.);
#4250=ORIENTED_EDGE('',*,*,#3186,.F.);
#4251=ORIENTED_EDGE('',*,*,#3187,.F.);
#4252=ORIENTED_EDGE('',*,*,#3188,.T.);
#4253=ORIENTED_EDGE('',*,*,#3105,.T.);
#4254=ORIENTED_EDGE('',*,*,#3188,.F.);
#4255=ORIENTED_EDGE('',*,*,#3189,.F.);
#4256=ORIENTED_EDGE('',*,*,#3190,.T.);
#4257=ORIENTED_EDGE('',*,*,#3101,.T.);
#4258=ORIENTED_EDGE('',*,*,#3190,.F.);
#4259=ORIENTED_EDGE('',*,*,#3191,.F.);
#4260=ORIENTED_EDGE('',*,*,#3182,.T.);
#4261=ORIENTED_EDGE('',*,*,#3183,.T.);
#4262=ORIENTED_EDGE('',*,*,#3191,.T.);
#4263=ORIENTED_EDGE('',*,*,#3189,.T.);
#4264=ORIENTED_EDGE('',*,*,#3187,.T.);
#4265=ORIENTED_EDGE('',*,*,#3185,.T.);
#4266=ORIENTED_EDGE('',*,*,#3097,.T.);
#4267=ORIENTED_EDGE('',*,*,#3192,.F.);
#4268=ORIENTED_EDGE('',*,*,#3193,.F.);
#4269=ORIENTED_EDGE('',*,*,#3194,.T.);
#4270=ORIENTED_EDGE('',*,*,#3098,.T.);
#4271=ORIENTED_EDGE('',*,*,#3194,.F.);
#4272=ORIENTED_EDGE('',*,*,#3195,.F.);
#4273=ORIENTED_EDGE('',*,*,#3196,.T.);
#4274=ORIENTED_EDGE('',*,*,#3099,.T.);
#4275=ORIENTED_EDGE('',*,*,#3196,.F.);
#4276=ORIENTED_EDGE('',*,*,#3197,.F.);
#4277=ORIENTED_EDGE('',*,*,#3198,.T.);
#4278=ORIENTED_EDGE('',*,*,#3100,.T.);
#4279=ORIENTED_EDGE('',*,*,#3198,.F.);
#4280=ORIENTED_EDGE('',*,*,#3199,.F.);
#4281=ORIENTED_EDGE('',*,*,#3200,.T.);
#4282=ORIENTED_EDGE('',*,*,#3096,.T.);
#4283=ORIENTED_EDGE('',*,*,#3200,.F.);
#4284=ORIENTED_EDGE('',*,*,#3201,.F.);
#4285=ORIENTED_EDGE('',*,*,#3192,.T.);
#4286=ORIENTED_EDGE('',*,*,#3193,.T.);
#4287=ORIENTED_EDGE('',*,*,#3201,.T.);
#4288=ORIENTED_EDGE('',*,*,#3199,.T.);
#4289=ORIENTED_EDGE('',*,*,#3197,.T.);
#4290=ORIENTED_EDGE('',*,*,#3195,.T.);
#4291=ORIENTED_EDGE('',*,*,#3202,.F.);
#4292=ORIENTED_EDGE('',*,*,#3203,.T.);
#4293=ORIENTED_EDGE('',*,*,#3204,.T.);
#4294=ORIENTED_EDGE('',*,*,#3203,.F.);
#4295=ORIENTED_EDGE('',*,*,#3205,.F.);
#4296=ORIENTED_EDGE('',*,*,#3206,.T.);
#4297=ORIENTED_EDGE('',*,*,#3207,.T.);
#4298=ORIENTED_EDGE('',*,*,#3206,.F.);
#4299=ORIENTED_EDGE('',*,*,#3208,.F.);
#4300=ORIENTED_EDGE('',*,*,#3209,.T.);
#4301=ORIENTED_EDGE('',*,*,#3210,.T.);
#4302=ORIENTED_EDGE('',*,*,#3209,.F.);
#4303=ORIENTED_EDGE('',*,*,#3211,.F.);
#4304=ORIENTED_EDGE('',*,*,#3212,.T.);
#4305=ORIENTED_EDGE('',*,*,#3213,.T.);
#4306=ORIENTED_EDGE('',*,*,#3212,.F.);
#4307=ORIENTED_EDGE('',*,*,#3214,.T.);
#4308=ORIENTED_EDGE('',*,*,#3215,.T.);
#4309=ORIENTED_EDGE('',*,*,#3216,.F.);
#4310=ORIENTED_EDGE('',*,*,#3215,.F.);
#4311=ORIENTED_EDGE('',*,*,#3217,.F.);
#4312=ORIENTED_EDGE('',*,*,#3218,.T.);
#4313=ORIENTED_EDGE('',*,*,#3219,.T.);
#4314=ORIENTED_EDGE('',*,*,#3220,.F.);
#4315=ORIENTED_EDGE('',*,*,#3202,.T.);
#4316=ORIENTED_EDGE('',*,*,#3216,.T.);
#4317=ORIENTED_EDGE('',*,*,#3208,.T.);
#4318=ORIENTED_EDGE('',*,*,#3214,.F.);
#4319=ORIENTED_EDGE('',*,*,#3221,.T.);
#4320=ORIENTED_EDGE('',*,*,#3222,.T.);
#4321=ORIENTED_EDGE('',*,*,#3223,.T.);
#4322=ORIENTED_EDGE('',*,*,#3224,.T.);
#4323=ORIENTED_EDGE('',*,*,#3225,.T.);
#4324=ORIENTED_EDGE('',*,*,#3226,.T.);
#4325=ORIENTED_EDGE('',*,*,#3227,.T.);
#4326=ORIENTED_EDGE('',*,*,#3228,.T.);
#4327=ORIENTED_EDGE('',*,*,#3229,.T.);
#4328=ORIENTED_EDGE('',*,*,#3230,.T.);
#4329=ORIENTED_EDGE('',*,*,#3231,.T.);
#4330=ORIENTED_EDGE('',*,*,#3232,.T.);
#4331=ORIENTED_EDGE('',*,*,#3233,.T.);
#4332=ORIENTED_EDGE('',*,*,#3234,.T.);
#4333=ORIENTED_EDGE('',*,*,#3235,.T.);
#4334=ORIENTED_EDGE('',*,*,#3236,.T.);
#4335=ORIENTED_EDGE('',*,*,#3237,.T.);
#4336=ORIENTED_EDGE('',*,*,#3238,.T.);
#4337=ORIENTED_EDGE('',*,*,#3239,.T.);
#4338=ORIENTED_EDGE('',*,*,#3240,.T.);
#4339=ORIENTED_EDGE('',*,*,#3241,.T.);
#4340=ORIENTED_EDGE('',*,*,#3242,.T.);
#4341=ORIENTED_EDGE('',*,*,#3243,.T.);
#4342=ORIENTED_EDGE('',*,*,#3244,.T.);
#4343=ORIENTED_EDGE('',*,*,#3245,.T.);
#4344=ORIENTED_EDGE('',*,*,#3246,.T.);
#4345=ORIENTED_EDGE('',*,*,#3247,.T.);
#4346=ORIENTED_EDGE('',*,*,#3248,.T.);
#4347=ORIENTED_EDGE('',*,*,#3249,.T.);
#4348=ORIENTED_EDGE('',*,*,#3250,.T.);
#4349=ORIENTED_EDGE('',*,*,#3251,.T.);
#4350=ORIENTED_EDGE('',*,*,#3252,.T.);
#4351=ORIENTED_EDGE('',*,*,#3253,.T.);
#4352=ORIENTED_EDGE('',*,*,#3254,.T.);
#4353=ORIENTED_EDGE('',*,*,#3255,.T.);
#4354=ORIENTED_EDGE('',*,*,#3217,.T.);
#4355=ORIENTED_EDGE('',*,*,#3256,.T.);
#4356=ORIENTED_EDGE('',*,*,#3257,.T.);
#4357=ORIENTED_EDGE('',*,*,#3258,.T.);
#4358=ORIENTED_EDGE('',*,*,#3259,.T.);
#4359=ORIENTED_EDGE('',*,*,#3260,.T.);
#4360=ORIENTED_EDGE('',*,*,#3261,.T.);
#4361=ORIENTED_EDGE('',*,*,#3262,.T.);
#4362=ORIENTED_EDGE('',*,*,#3263,.T.);
#4363=ORIENTED_EDGE('',*,*,#3264,.T.);
#4364=ORIENTED_EDGE('',*,*,#3265,.T.);
#4365=ORIENTED_EDGE('',*,*,#3266,.T.);
#4366=ORIENTED_EDGE('',*,*,#3267,.T.);
#4367=ORIENTED_EDGE('',*,*,#3268,.T.);
#4368=ORIENTED_EDGE('',*,*,#3269,.T.);
#4369=ORIENTED_EDGE('',*,*,#3270,.T.);
#4370=ORIENTED_EDGE('',*,*,#3271,.T.);
#4371=ORIENTED_EDGE('',*,*,#3272,.T.);
#4372=ORIENTED_EDGE('',*,*,#3273,.T.);
#4373=ORIENTED_EDGE('',*,*,#3274,.T.);
#4374=ORIENTED_EDGE('',*,*,#3275,.T.);
#4375=ORIENTED_EDGE('',*,*,#3276,.T.);
#4376=ORIENTED_EDGE('',*,*,#3277,.T.);
#4377=ORIENTED_EDGE('',*,*,#3278,.T.);
#4378=ORIENTED_EDGE('',*,*,#3279,.T.);
#4379=ORIENTED_EDGE('',*,*,#3280,.T.);
#4380=ORIENTED_EDGE('',*,*,#3281,.T.);
#4381=ORIENTED_EDGE('',*,*,#3282,.T.);
#4382=ORIENTED_EDGE('',*,*,#3283,.T.);
#4383=ORIENTED_EDGE('',*,*,#3284,.T.);
#4384=ORIENTED_EDGE('',*,*,#3285,.T.);
#4385=ORIENTED_EDGE('',*,*,#3286,.T.);
#4386=ORIENTED_EDGE('',*,*,#3287,.T.);
#4387=ORIENTED_EDGE('',*,*,#3288,.T.);
#4388=ORIENTED_EDGE('',*,*,#3289,.T.);
#4389=ORIENTED_EDGE('',*,*,#3290,.T.);
#4390=ORIENTED_EDGE('',*,*,#3291,.T.);
#4391=ORIENTED_EDGE('',*,*,#3292,.T.);
#4392=ORIENTED_EDGE('',*,*,#3293,.T.);
#4393=ORIENTED_EDGE('',*,*,#3294,.T.);
#4394=ORIENTED_EDGE('',*,*,#3295,.T.);
#4395=ORIENTED_EDGE('',*,*,#3296,.T.);
#4396=ORIENTED_EDGE('',*,*,#3297,.T.);
#4397=ORIENTED_EDGE('',*,*,#3298,.T.);
#4398=ORIENTED_EDGE('',*,*,#3299,.T.);
#4399=ORIENTED_EDGE('',*,*,#3213,.F.);
#4400=ORIENTED_EDGE('',*,*,#3300,.F.);
#4401=ORIENTED_EDGE('',*,*,#3301,.F.);
#4402=ORIENTED_EDGE('',*,*,#3302,.F.);
#4403=ORIENTED_EDGE('',*,*,#3303,.F.);
#4404=ORIENTED_EDGE('',*,*,#3304,.F.);
#4405=ORIENTED_EDGE('',*,*,#3305,.F.);
#4406=ORIENTED_EDGE('',*,*,#3306,.F.);
#4407=ORIENTED_EDGE('',*,*,#3307,.F.);
#4408=ORIENTED_EDGE('',*,*,#3308,.F.);
#4409=ORIENTED_EDGE('',*,*,#3309,.F.);
#4410=ORIENTED_EDGE('',*,*,#3310,.F.);
#4411=ORIENTED_EDGE('',*,*,#3311,.F.);
#4412=ORIENTED_EDGE('',*,*,#3312,.F.);
#4413=ORIENTED_EDGE('',*,*,#3313,.F.);
#4414=ORIENTED_EDGE('',*,*,#3314,.F.);
#4415=ORIENTED_EDGE('',*,*,#3315,.F.);
#4416=ORIENTED_EDGE('',*,*,#3316,.F.);
#4417=ORIENTED_EDGE('',*,*,#3317,.F.);
#4418=ORIENTED_EDGE('',*,*,#3318,.F.);
#4419=ORIENTED_EDGE('',*,*,#3319,.F.);
#4420=ORIENTED_EDGE('',*,*,#3320,.F.);
#4421=ORIENTED_EDGE('',*,*,#3321,.F.);
#4422=ORIENTED_EDGE('',*,*,#3322,.F.);
#4423=ORIENTED_EDGE('',*,*,#3323,.F.);
#4424=ORIENTED_EDGE('',*,*,#3324,.F.);
#4425=ORIENTED_EDGE('',*,*,#3325,.F.);
#4426=ORIENTED_EDGE('',*,*,#3326,.F.);
#4427=ORIENTED_EDGE('',*,*,#3327,.F.);
#4428=ORIENTED_EDGE('',*,*,#3328,.F.);
#4429=ORIENTED_EDGE('',*,*,#3329,.F.);
#4430=ORIENTED_EDGE('',*,*,#3330,.F.);
#4431=ORIENTED_EDGE('',*,*,#3331,.F.);
#4432=ORIENTED_EDGE('',*,*,#3332,.F.);
#4433=ORIENTED_EDGE('',*,*,#3333,.F.);
#4434=ORIENTED_EDGE('',*,*,#3334,.F.);
#4435=ORIENTED_EDGE('',*,*,#3335,.F.);
#4436=ORIENTED_EDGE('',*,*,#3336,.F.);
#4437=ORIENTED_EDGE('',*,*,#3337,.F.);
#4438=ORIENTED_EDGE('',*,*,#3338,.F.);
#4439=ORIENTED_EDGE('',*,*,#3339,.F.);
#4440=ORIENTED_EDGE('',*,*,#3340,.F.);
#4441=ORIENTED_EDGE('',*,*,#3341,.F.);
#4442=ORIENTED_EDGE('',*,*,#3342,.F.);
#4443=ORIENTED_EDGE('',*,*,#3343,.F.);
#4444=ORIENTED_EDGE('',*,*,#3344,.F.);
#4445=ORIENTED_EDGE('',*,*,#3219,.F.);
#4446=ORIENTED_EDGE('',*,*,#3345,.F.);
#4447=ORIENTED_EDGE('',*,*,#3346,.F.);
#4448=ORIENTED_EDGE('',*,*,#3347,.F.);
#4449=ORIENTED_EDGE('',*,*,#3348,.F.);
#4450=ORIENTED_EDGE('',*,*,#3349,.F.);
#4451=ORIENTED_EDGE('',*,*,#3350,.F.);
#4452=ORIENTED_EDGE('',*,*,#3351,.F.);
#4453=ORIENTED_EDGE('',*,*,#3352,.F.);
#4454=ORIENTED_EDGE('',*,*,#3353,.F.);
#4455=ORIENTED_EDGE('',*,*,#3354,.F.);
#4456=ORIENTED_EDGE('',*,*,#3355,.F.);
#4457=ORIENTED_EDGE('',*,*,#3356,.F.);
#4458=ORIENTED_EDGE('',*,*,#3357,.F.);
#4459=ORIENTED_EDGE('',*,*,#3358,.F.);
#4460=ORIENTED_EDGE('',*,*,#3359,.F.);
#4461=ORIENTED_EDGE('',*,*,#3360,.F.);
#4462=ORIENTED_EDGE('',*,*,#3361,.F.);
#4463=ORIENTED_EDGE('',*,*,#3362,.F.);
#4464=ORIENTED_EDGE('',*,*,#3363,.F.);
#4465=ORIENTED_EDGE('',*,*,#3364,.F.);
#4466=ORIENTED_EDGE('',*,*,#3365,.F.);
#4467=ORIENTED_EDGE('',*,*,#3366,.F.);
#4468=ORIENTED_EDGE('',*,*,#3367,.F.);
#4469=ORIENTED_EDGE('',*,*,#3368,.F.);
#4470=ORIENTED_EDGE('',*,*,#3369,.F.);
#4471=ORIENTED_EDGE('',*,*,#3370,.F.);
#4472=ORIENTED_EDGE('',*,*,#3371,.F.);
#4473=ORIENTED_EDGE('',*,*,#3372,.F.);
#4474=ORIENTED_EDGE('',*,*,#3373,.F.);
#4475=ORIENTED_EDGE('',*,*,#3374,.F.);
#4476=ORIENTED_EDGE('',*,*,#3375,.F.);
#4477=ORIENTED_EDGE('',*,*,#3376,.F.);
#4478=ORIENTED_EDGE('',*,*,#3377,.F.);
#4479=ORIENTED_EDGE('',*,*,#3378,.F.);
#4480=ORIENTED_EDGE('',*,*,#3207,.F.);
#4481=ORIENTED_EDGE('',*,*,#3300,.T.);
#4482=ORIENTED_EDGE('',*,*,#3379,.F.);
#4483=ORIENTED_EDGE('',*,*,#3221,.F.);
#4484=ORIENTED_EDGE('',*,*,#3380,.T.);
#4485=ORIENTED_EDGE('',*,*,#3378,.T.);
#4486=ORIENTED_EDGE('',*,*,#3381,.F.);
#4487=ORIENTED_EDGE('',*,*,#3222,.F.);
#4488=ORIENTED_EDGE('',*,*,#3379,.T.);
#4489=ORIENTED_EDGE('',*,*,#3377,.T.);
#4490=ORIENTED_EDGE('',*,*,#3382,.F.);
#4491=ORIENTED_EDGE('',*,*,#3223,.F.);
#4492=ORIENTED_EDGE('',*,*,#3381,.T.);
#4493=ORIENTED_EDGE('',*,*,#3376,.T.);
#4494=ORIENTED_EDGE('',*,*,#3383,.F.);
#4495=ORIENTED_EDGE('',*,*,#3224,.F.);
#4496=ORIENTED_EDGE('',*,*,#3382,.T.);
#4497=ORIENTED_EDGE('',*,*,#3375,.T.);
#4498=ORIENTED_EDGE('',*,*,#3384,.F.);
#4499=ORIENTED_EDGE('',*,*,#3225,.F.);
#4500=ORIENTED_EDGE('',*,*,#3383,.T.);
#4501=ORIENTED_EDGE('',*,*,#3374,.T.);
#4502=ORIENTED_EDGE('',*,*,#3385,.F.);
#4503=ORIENTED_EDGE('',*,*,#3226,.F.);
#4504=ORIENTED_EDGE('',*,*,#3384,.T.);
#4505=ORIENTED_EDGE('',*,*,#3373,.T.);
#4506=ORIENTED_EDGE('',*,*,#3386,.F.);
#4507=ORIENTED_EDGE('',*,*,#3227,.F.);
#4508=ORIENTED_EDGE('',*,*,#3385,.T.);
#4509=ORIENTED_EDGE('',*,*,#3372,.T.);
#4510=ORIENTED_EDGE('',*,*,#3387,.F.);
#4511=ORIENTED_EDGE('',*,*,#3228,.F.);
#4512=ORIENTED_EDGE('',*,*,#3386,.T.);
#4513=ORIENTED_EDGE('',*,*,#3371,.T.);
#4514=ORIENTED_EDGE('',*,*,#3388,.F.);
#4515=ORIENTED_EDGE('',*,*,#3229,.F.);
#4516=ORIENTED_EDGE('',*,*,#3387,.T.);
#4517=ORIENTED_EDGE('',*,*,#3370,.T.);
#4518=ORIENTED_EDGE('',*,*,#3389,.F.);
#4519=ORIENTED_EDGE('',*,*,#3230,.F.);
#4520=ORIENTED_EDGE('',*,*,#3388,.T.);
#4521=ORIENTED_EDGE('',*,*,#3369,.T.);
#4522=ORIENTED_EDGE('',*,*,#3390,.F.);
#4523=ORIENTED_EDGE('',*,*,#3231,.F.);
#4524=ORIENTED_EDGE('',*,*,#3389,.T.);
#4525=ORIENTED_EDGE('',*,*,#3368,.T.);
#4526=ORIENTED_EDGE('',*,*,#3391,.F.);
#4527=ORIENTED_EDGE('',*,*,#3232,.F.);
#4528=ORIENTED_EDGE('',*,*,#3390,.T.);
#4529=ORIENTED_EDGE('',*,*,#3367,.T.);
#4530=ORIENTED_EDGE('',*,*,#3392,.F.);
#4531=ORIENTED_EDGE('',*,*,#3233,.F.);
#4532=ORIENTED_EDGE('',*,*,#3391,.T.);
#4533=ORIENTED_EDGE('',*,*,#3366,.T.);
#4534=ORIENTED_EDGE('',*,*,#3393,.F.);
#4535=ORIENTED_EDGE('',*,*,#3234,.F.);
#4536=ORIENTED_EDGE('',*,*,#3392,.T.);
#4537=ORIENTED_EDGE('',*,*,#3365,.T.);
#4538=ORIENTED_EDGE('',*,*,#3394,.F.);
#4539=ORIENTED_EDGE('',*,*,#3235,.F.);
#4540=ORIENTED_EDGE('',*,*,#3393,.T.);
#4541=ORIENTED_EDGE('',*,*,#3364,.T.);
#4542=ORIENTED_EDGE('',*,*,#3395,.F.);
#4543=ORIENTED_EDGE('',*,*,#3236,.F.);
#4544=ORIENTED_EDGE('',*,*,#3394,.T.);
#4545=ORIENTED_EDGE('',*,*,#3363,.T.);
#4546=ORIENTED_EDGE('',*,*,#3396,.F.);
#4547=ORIENTED_EDGE('',*,*,#3237,.F.);
#4548=ORIENTED_EDGE('',*,*,#3395,.T.);
#4549=ORIENTED_EDGE('',*,*,#3362,.T.);
#4550=ORIENTED_EDGE('',*,*,#3397,.F.);
#4551=ORIENTED_EDGE('',*,*,#3238,.F.);
#4552=ORIENTED_EDGE('',*,*,#3396,.T.);
#4553=ORIENTED_EDGE('',*,*,#3361,.T.);
#4554=ORIENTED_EDGE('',*,*,#3398,.F.);
#4555=ORIENTED_EDGE('',*,*,#3239,.F.);
#4556=ORIENTED_EDGE('',*,*,#3397,.T.);
#4557=ORIENTED_EDGE('',*,*,#3360,.T.);
#4558=ORIENTED_EDGE('',*,*,#3399,.F.);
#4559=ORIENTED_EDGE('',*,*,#3240,.F.);
#4560=ORIENTED_EDGE('',*,*,#3398,.T.);
#4561=ORIENTED_EDGE('',*,*,#3359,.T.);
#4562=ORIENTED_EDGE('',*,*,#3400,.F.);
#4563=ORIENTED_EDGE('',*,*,#3241,.F.);
#4564=ORIENTED_EDGE('',*,*,#3399,.T.);
#4565=ORIENTED_EDGE('',*,*,#3358,.T.);
#4566=ORIENTED_EDGE('',*,*,#3401,.F.);
#4567=ORIENTED_EDGE('',*,*,#3242,.F.);
#4568=ORIENTED_EDGE('',*,*,#3400,.T.);
#4569=ORIENTED_EDGE('',*,*,#3357,.T.);
#4570=ORIENTED_EDGE('',*,*,#3402,.F.);
#4571=ORIENTED_EDGE('',*,*,#3243,.F.);
#4572=ORIENTED_EDGE('',*,*,#3401,.T.);
#4573=ORIENTED_EDGE('',*,*,#3356,.T.);
#4574=ORIENTED_EDGE('',*,*,#3403,.F.);
#4575=ORIENTED_EDGE('',*,*,#3244,.F.);
#4576=ORIENTED_EDGE('',*,*,#3402,.T.);
#4577=ORIENTED_EDGE('',*,*,#3355,.T.);
#4578=ORIENTED_EDGE('',*,*,#3404,.F.);
#4579=ORIENTED_EDGE('',*,*,#3245,.F.);
#4580=ORIENTED_EDGE('',*,*,#3403,.T.);
#4581=ORIENTED_EDGE('',*,*,#3354,.T.);
#4582=ORIENTED_EDGE('',*,*,#3405,.F.);
#4583=ORIENTED_EDGE('',*,*,#3246,.F.);
#4584=ORIENTED_EDGE('',*,*,#3404,.T.);
#4585=ORIENTED_EDGE('',*,*,#3353,.T.);
#4586=ORIENTED_EDGE('',*,*,#3406,.F.);
#4587=ORIENTED_EDGE('',*,*,#3247,.F.);
#4588=ORIENTED_EDGE('',*,*,#3405,.T.);
#4589=ORIENTED_EDGE('',*,*,#3352,.T.);
#4590=ORIENTED_EDGE('',*,*,#3407,.F.);
#4591=ORIENTED_EDGE('',*,*,#3248,.F.);
#4592=ORIENTED_EDGE('',*,*,#3406,.T.);
#4593=ORIENTED_EDGE('',*,*,#3351,.T.);
#4594=ORIENTED_EDGE('',*,*,#3408,.F.);
#4595=ORIENTED_EDGE('',*,*,#3249,.F.);
#4596=ORIENTED_EDGE('',*,*,#3407,.T.);
#4597=ORIENTED_EDGE('',*,*,#3350,.T.);
#4598=ORIENTED_EDGE('',*,*,#3409,.F.);
#4599=ORIENTED_EDGE('',*,*,#3250,.F.);
#4600=ORIENTED_EDGE('',*,*,#3408,.T.);
#4601=ORIENTED_EDGE('',*,*,#3349,.T.);
#4602=ORIENTED_EDGE('',*,*,#3410,.F.);
#4603=ORIENTED_EDGE('',*,*,#3251,.F.);
#4604=ORIENTED_EDGE('',*,*,#3409,.T.);
#4605=ORIENTED_EDGE('',*,*,#3348,.T.);
#4606=ORIENTED_EDGE('',*,*,#3411,.F.);
#4607=ORIENTED_EDGE('',*,*,#3252,.F.);
#4608=ORIENTED_EDGE('',*,*,#3410,.T.);
#4609=ORIENTED_EDGE('',*,*,#3347,.T.);
#4610=ORIENTED_EDGE('',*,*,#3412,.F.);
#4611=ORIENTED_EDGE('',*,*,#3253,.F.);
#4612=ORIENTED_EDGE('',*,*,#3411,.T.);
#4613=ORIENTED_EDGE('',*,*,#3346,.T.);
#4614=ORIENTED_EDGE('',*,*,#3413,.F.);
#4615=ORIENTED_EDGE('',*,*,#3254,.F.);
#4616=ORIENTED_EDGE('',*,*,#3412,.T.);
#4617=ORIENTED_EDGE('',*,*,#3345,.T.);
#4618=ORIENTED_EDGE('',*,*,#3218,.F.);
#4619=ORIENTED_EDGE('',*,*,#3255,.F.);
#4620=ORIENTED_EDGE('',*,*,#3413,.T.);
#4621=ORIENTED_EDGE('',*,*,#3344,.T.);
#4622=ORIENTED_EDGE('',*,*,#3414,.F.);
#4623=ORIENTED_EDGE('',*,*,#3256,.F.);
#4624=ORIENTED_EDGE('',*,*,#3220,.T.);
#4625=ORIENTED_EDGE('',*,*,#3343,.T.);
#4626=ORIENTED_EDGE('',*,*,#3415,.F.);
#4627=ORIENTED_EDGE('',*,*,#3257,.F.);
#4628=ORIENTED_EDGE('',*,*,#3414,.T.);
#4629=ORIENTED_EDGE('',*,*,#3342,.T.);
#4630=ORIENTED_EDGE('',*,*,#3416,.F.);
#4631=ORIENTED_EDGE('',*,*,#3258,.F.);
#4632=ORIENTED_EDGE('',*,*,#3415,.T.);
#4633=ORIENTED_EDGE('',*,*,#3341,.T.);
#4634=ORIENTED_EDGE('',*,*,#3417,.F.);
#4635=ORIENTED_EDGE('',*,*,#3259,.F.);
#4636=ORIENTED_EDGE('',*,*,#3416,.T.);
#4637=ORIENTED_EDGE('',*,*,#3340,.T.);
#4638=ORIENTED_EDGE('',*,*,#3418,.F.);
#4639=ORIENTED_EDGE('',*,*,#3260,.F.);
#4640=ORIENTED_EDGE('',*,*,#3417,.T.);
#4641=ORIENTED_EDGE('',*,*,#3339,.T.);
#4642=ORIENTED_EDGE('',*,*,#3419,.F.);
#4643=ORIENTED_EDGE('',*,*,#3261,.F.);
#4644=ORIENTED_EDGE('',*,*,#3418,.T.);
#4645=ORIENTED_EDGE('',*,*,#3338,.T.);
#4646=ORIENTED_EDGE('',*,*,#3420,.F.);
#4647=ORIENTED_EDGE('',*,*,#3262,.F.);
#4648=ORIENTED_EDGE('',*,*,#3419,.T.);
#4649=ORIENTED_EDGE('',*,*,#3337,.T.);
#4650=ORIENTED_EDGE('',*,*,#3421,.F.);
#4651=ORIENTED_EDGE('',*,*,#3263,.F.);
#4652=ORIENTED_EDGE('',*,*,#3420,.T.);
#4653=ORIENTED_EDGE('',*,*,#3336,.T.);
#4654=ORIENTED_EDGE('',*,*,#3422,.F.);
#4655=ORIENTED_EDGE('',*,*,#3264,.F.);
#4656=ORIENTED_EDGE('',*,*,#3421,.T.);
#4657=ORIENTED_EDGE('',*,*,#3335,.T.);
#4658=ORIENTED_EDGE('',*,*,#3423,.F.);
#4659=ORIENTED_EDGE('',*,*,#3265,.F.);
#4660=ORIENTED_EDGE('',*,*,#3422,.T.);
#4661=ORIENTED_EDGE('',*,*,#3334,.T.);
#4662=ORIENTED_EDGE('',*,*,#3424,.F.);
#4663=ORIENTED_EDGE('',*,*,#3266,.F.);
#4664=ORIENTED_EDGE('',*,*,#3423,.T.);
#4665=ORIENTED_EDGE('',*,*,#3333,.T.);
#4666=ORIENTED_EDGE('',*,*,#3425,.F.);
#4667=ORIENTED_EDGE('',*,*,#3267,.F.);
#4668=ORIENTED_EDGE('',*,*,#3424,.T.);
#4669=ORIENTED_EDGE('',*,*,#3332,.T.);
#4670=ORIENTED_EDGE('',*,*,#3426,.F.);
#4671=ORIENTED_EDGE('',*,*,#3268,.F.);
#4672=ORIENTED_EDGE('',*,*,#3425,.T.);
#4673=ORIENTED_EDGE('',*,*,#3331,.T.);
#4674=ORIENTED_EDGE('',*,*,#3427,.F.);
#4675=ORIENTED_EDGE('',*,*,#3269,.F.);
#4676=ORIENTED_EDGE('',*,*,#3426,.T.);
#4677=ORIENTED_EDGE('',*,*,#3330,.T.);
#4678=ORIENTED_EDGE('',*,*,#3428,.F.);
#4679=ORIENTED_EDGE('',*,*,#3270,.F.);
#4680=ORIENTED_EDGE('',*,*,#3427,.T.);
#4681=ORIENTED_EDGE('',*,*,#3329,.T.);
#4682=ORIENTED_EDGE('',*,*,#3429,.F.);
#4683=ORIENTED_EDGE('',*,*,#3271,.F.);
#4684=ORIENTED_EDGE('',*,*,#3428,.T.);
#4685=ORIENTED_EDGE('',*,*,#3328,.T.);
#4686=ORIENTED_EDGE('',*,*,#3430,.F.);
#4687=ORIENTED_EDGE('',*,*,#3272,.F.);
#4688=ORIENTED_EDGE('',*,*,#3429,.T.);
#4689=ORIENTED_EDGE('',*,*,#3327,.T.);
#4690=ORIENTED_EDGE('',*,*,#3431,.F.);
#4691=ORIENTED_EDGE('',*,*,#3273,.F.);
#4692=ORIENTED_EDGE('',*,*,#3430,.T.);
#4693=ORIENTED_EDGE('',*,*,#3326,.T.);
#4694=ORIENTED_EDGE('',*,*,#3432,.F.);
#4695=ORIENTED_EDGE('',*,*,#3274,.F.);
#4696=ORIENTED_EDGE('',*,*,#3431,.T.);
#4697=ORIENTED_EDGE('',*,*,#3325,.T.);
#4698=ORIENTED_EDGE('',*,*,#3433,.F.);
#4699=ORIENTED_EDGE('',*,*,#3275,.F.);
#4700=ORIENTED_EDGE('',*,*,#3432,.T.);
#4701=ORIENTED_EDGE('',*,*,#3324,.T.);
#4702=ORIENTED_EDGE('',*,*,#3434,.F.);
#4703=ORIENTED_EDGE('',*,*,#3276,.F.);
#4704=ORIENTED_EDGE('',*,*,#3433,.T.);
#4705=ORIENTED_EDGE('',*,*,#3323,.T.);
#4706=ORIENTED_EDGE('',*,*,#3435,.F.);
#4707=ORIENTED_EDGE('',*,*,#3277,.F.);
#4708=ORIENTED_EDGE('',*,*,#3434,.T.);
#4709=ORIENTED_EDGE('',*,*,#3322,.T.);
#4710=ORIENTED_EDGE('',*,*,#3436,.F.);
#4711=ORIENTED_EDGE('',*,*,#3278,.F.);
#4712=ORIENTED_EDGE('',*,*,#3435,.T.);
#4713=ORIENTED_EDGE('',*,*,#3321,.T.);
#4714=ORIENTED_EDGE('',*,*,#3437,.F.);
#4715=ORIENTED_EDGE('',*,*,#3279,.F.);
#4716=ORIENTED_EDGE('',*,*,#3436,.T.);
#4717=ORIENTED_EDGE('',*,*,#3320,.T.);
#4718=ORIENTED_EDGE('',*,*,#3438,.F.);
#4719=ORIENTED_EDGE('',*,*,#3280,.F.);
#4720=ORIENTED_EDGE('',*,*,#3437,.T.);
#4721=ORIENTED_EDGE('',*,*,#3319,.T.);
#4722=ORIENTED_EDGE('',*,*,#3439,.F.);
#4723=ORIENTED_EDGE('',*,*,#3281,.F.);
#4724=ORIENTED_EDGE('',*,*,#3438,.T.);
#4725=ORIENTED_EDGE('',*,*,#3318,.T.);
#4726=ORIENTED_EDGE('',*,*,#3440,.F.);
#4727=ORIENTED_EDGE('',*,*,#3282,.F.);
#4728=ORIENTED_EDGE('',*,*,#3439,.T.);
#4729=ORIENTED_EDGE('',*,*,#3317,.T.);
#4730=ORIENTED_EDGE('',*,*,#3441,.F.);
#4731=ORIENTED_EDGE('',*,*,#3283,.F.);
#4732=ORIENTED_EDGE('',*,*,#3440,.T.);
#4733=ORIENTED_EDGE('',*,*,#3316,.T.);
#4734=ORIENTED_EDGE('',*,*,#3442,.F.);
#4735=ORIENTED_EDGE('',*,*,#3284,.F.);
#4736=ORIENTED_EDGE('',*,*,#3441,.T.);
#4737=ORIENTED_EDGE('',*,*,#3315,.T.);
#4738=ORIENTED_EDGE('',*,*,#3443,.F.);
#4739=ORIENTED_EDGE('',*,*,#3285,.F.);
#4740=ORIENTED_EDGE('',*,*,#3442,.T.);
#4741=ORIENTED_EDGE('',*,*,#3314,.T.);
#4742=ORIENTED_EDGE('',*,*,#3444,.F.);
#4743=ORIENTED_EDGE('',*,*,#3286,.F.);
#4744=ORIENTED_EDGE('',*,*,#3443,.T.);
#4745=ORIENTED_EDGE('',*,*,#3313,.T.);
#4746=ORIENTED_EDGE('',*,*,#3445,.F.);
#4747=ORIENTED_EDGE('',*,*,#3287,.F.);
#4748=ORIENTED_EDGE('',*,*,#3444,.T.);
#4749=ORIENTED_EDGE('',*,*,#3312,.T.);
#4750=ORIENTED_EDGE('',*,*,#3446,.F.);
#4751=ORIENTED_EDGE('',*,*,#3288,.F.);
#4752=ORIENTED_EDGE('',*,*,#3445,.T.);
#4753=ORIENTED_EDGE('',*,*,#3311,.T.);
#4754=ORIENTED_EDGE('',*,*,#3447,.F.);
#4755=ORIENTED_EDGE('',*,*,#3289,.F.);
#4756=ORIENTED_EDGE('',*,*,#3446,.T.);
#4757=ORIENTED_EDGE('',*,*,#3310,.T.);
#4758=ORIENTED_EDGE('',*,*,#3448,.F.);
#4759=ORIENTED_EDGE('',*,*,#3290,.F.);
#4760=ORIENTED_EDGE('',*,*,#3447,.T.);
#4761=ORIENTED_EDGE('',*,*,#3309,.T.);
#4762=ORIENTED_EDGE('',*,*,#3449,.F.);
#4763=ORIENTED_EDGE('',*,*,#3291,.F.);
#4764=ORIENTED_EDGE('',*,*,#3448,.T.);
#4765=ORIENTED_EDGE('',*,*,#3308,.T.);
#4766=ORIENTED_EDGE('',*,*,#3450,.F.);
#4767=ORIENTED_EDGE('',*,*,#3292,.F.);
#4768=ORIENTED_EDGE('',*,*,#3449,.T.);
#4769=ORIENTED_EDGE('',*,*,#3307,.T.);
#4770=ORIENTED_EDGE('',*,*,#3451,.F.);
#4771=ORIENTED_EDGE('',*,*,#3293,.F.);
#4772=ORIENTED_EDGE('',*,*,#3450,.T.);
#4773=ORIENTED_EDGE('',*,*,#3306,.T.);
#4774=ORIENTED_EDGE('',*,*,#3452,.F.);
#4775=ORIENTED_EDGE('',*,*,#3294,.F.);
#4776=ORIENTED_EDGE('',*,*,#3451,.T.);
#4777=ORIENTED_EDGE('',*,*,#3305,.T.);
#4778=ORIENTED_EDGE('',*,*,#3453,.F.);
#4779=ORIENTED_EDGE('',*,*,#3295,.F.);
#4780=ORIENTED_EDGE('',*,*,#3452,.T.);
#4781=ORIENTED_EDGE('',*,*,#3304,.T.);
#4782=ORIENTED_EDGE('',*,*,#3454,.F.);
#4783=ORIENTED_EDGE('',*,*,#3296,.F.);
#4784=ORIENTED_EDGE('',*,*,#3453,.T.);
#4785=ORIENTED_EDGE('',*,*,#3303,.T.);
#4786=ORIENTED_EDGE('',*,*,#3455,.F.);
#4787=ORIENTED_EDGE('',*,*,#3297,.F.);
#4788=ORIENTED_EDGE('',*,*,#3454,.T.);
#4789=ORIENTED_EDGE('',*,*,#3302,.T.);
#4790=ORIENTED_EDGE('',*,*,#3456,.F.);
#4791=ORIENTED_EDGE('',*,*,#3298,.F.);
#4792=ORIENTED_EDGE('',*,*,#3455,.T.);
#4793=ORIENTED_EDGE('',*,*,#3301,.T.);
#4794=ORIENTED_EDGE('',*,*,#3380,.F.);
#4795=ORIENTED_EDGE('',*,*,#3299,.F.);
#4796=ORIENTED_EDGE('',*,*,#3456,.T.);
#4797=ORIENTED_EDGE('',*,*,#3211,.T.);
#4798=ORIENTED_EDGE('',*,*,#3210,.F.);
#4799=ORIENTED_EDGE('',*,*,#3205,.T.);
#4800=ORIENTED_EDGE('',*,*,#3204,.F.);
#4801=ORIENTED_EDGE('',*,*,#3457,.T.);
#4802=ORIENTED_EDGE('',*,*,#3458,.T.);
#4803=ORIENTED_EDGE('',*,*,#3459,.F.);
#4804=ORIENTED_EDGE('',*,*,#3458,.F.);
#4805=ORIENTED_EDGE('',*,*,#3460,.T.);
#4806=ORIENTED_EDGE('',*,*,#3461,.T.);
#4807=ORIENTED_EDGE('',*,*,#3462,.F.);
#4808=ORIENTED_EDGE('',*,*,#3461,.F.);
#4809=ORIENTED_EDGE('',*,*,#3463,.T.);
#4810=ORIENTED_EDGE('',*,*,#3464,.T.);
#4811=ORIENTED_EDGE('',*,*,#3465,.T.);
#4812=ORIENTED_EDGE('',*,*,#3466,.T.);
#4813=ORIENTED_EDGE('',*,*,#3457,.F.);
#4814=ORIENTED_EDGE('',*,*,#3460,.F.);
#4815=ORIENTED_EDGE('',*,*,#3467,.F.);
#4816=ORIENTED_EDGE('',*,*,#3468,.F.);
#4817=ORIENTED_EDGE('',*,*,#3469,.F.);
#4818=ORIENTED_EDGE('',*,*,#3470,.F.);
#4819=ORIENTED_EDGE('',*,*,#3459,.T.);
#4820=ORIENTED_EDGE('',*,*,#3462,.T.);
#4821=ORIENTED_EDGE('',*,*,#3467,.T.);
#4822=ORIENTED_EDGE('',*,*,#3471,.F.);
#4823=ORIENTED_EDGE('',*,*,#3463,.F.);
#4824=ORIENTED_EDGE('',*,*,#3472,.T.);
#4825=ORIENTED_EDGE('',*,*,#3470,.T.);
#4826=ORIENTED_EDGE('',*,*,#3473,.F.);
#4827=ORIENTED_EDGE('',*,*,#3464,.F.);
#4828=ORIENTED_EDGE('',*,*,#3471,.T.);
#4829=ORIENTED_EDGE('',*,*,#3469,.T.);
#4830=ORIENTED_EDGE('',*,*,#3474,.F.);
#4831=ORIENTED_EDGE('',*,*,#3465,.F.);
#4832=ORIENTED_EDGE('',*,*,#3473,.T.);
#4833=ORIENTED_EDGE('',*,*,#3468,.T.);
#4834=ORIENTED_EDGE('',*,*,#3472,.F.);
#4835=ORIENTED_EDGE('',*,*,#3466,.F.);
#4836=ORIENTED_EDGE('',*,*,#3474,.T.);
#4837=ORIENTED_EDGE('',*,*,#3475,.T.);
#4838=ORIENTED_EDGE('',*,*,#3476,.T.);
#4839=ORIENTED_EDGE('',*,*,#3477,.T.);
#4840=ORIENTED_EDGE('',*,*,#3478,.T.);
#4841=ORIENTED_EDGE('',*,*,#3479,.T.);
#4842=ORIENTED_EDGE('',*,*,#3480,.T.);
#4843=ORIENTED_EDGE('',*,*,#3481,.T.);
#4844=ORIENTED_EDGE('',*,*,#3475,.F.);
#4845=ORIENTED_EDGE('',*,*,#3482,.F.);
#4846=ORIENTED_EDGE('',*,*,#3483,.T.);
#4847=ORIENTED_EDGE('',*,*,#3484,.F.);
#4848=ORIENTED_EDGE('',*,*,#3483,.F.);
#4849=ORIENTED_EDGE('',*,*,#3485,.F.);
#4850=ORIENTED_EDGE('',*,*,#3486,.T.);
#4851=ORIENTED_EDGE('',*,*,#3487,.T.);
#4852=ORIENTED_EDGE('',*,*,#3486,.F.);
#4853=ORIENTED_EDGE('',*,*,#3484,.T.);
#4854=ORIENTED_EDGE('',*,*,#3488,.T.);
#4855=ORIENTED_EDGE('',*,*,#3485,.T.);
#4856=ORIENTED_EDGE('',*,*,#3488,.F.);
#4857=ORIENTED_EDGE('',*,*,#3489,.F.);
#4858=ORIENTED_EDGE('',*,*,#3490,.T.);
#4859=ORIENTED_EDGE('',*,*,#3491,.T.);
#4860=ORIENTED_EDGE('',*,*,#3490,.F.);
#4861=ORIENTED_EDGE('',*,*,#3489,.T.);
#4862=ORIENTED_EDGE('',*,*,#3492,.F.);
#4863=ORIENTED_EDGE('',*,*,#3492,.T.);
#4864=ORIENTED_EDGE('',*,*,#3493,.T.);
#4865=ORIENTED_EDGE('',*,*,#3494,.T.);
#4866=ORIENTED_EDGE('',*,*,#3495,.T.);
#4867=ORIENTED_EDGE('',*,*,#3496,.T.);
#4868=ORIENTED_EDGE('',*,*,#3497,.T.);
#4869=ORIENTED_EDGE('',*,*,#3498,.T.);
#4870=ORIENTED_EDGE('',*,*,#3491,.F.);
#4871=ORIENTED_EDGE('',*,*,#3482,.T.);
#4872=ORIENTED_EDGE('',*,*,#3487,.F.);
#4873=ORIENTED_EDGE('',*,*,#3499,.T.);
#4874=ORIENTED_EDGE('',*,*,#3500,.T.);
#4875=ORIENTED_EDGE('',*,*,#3501,.T.);
#4876=ORIENTED_EDGE('',*,*,#3494,.F.);
#4877=ORIENTED_EDGE('',*,*,#3502,.F.);
#4878=ORIENTED_EDGE('',*,*,#3503,.T.);
#4879=ORIENTED_EDGE('',*,*,#3504,.T.);
#4880=ORIENTED_EDGE('',*,*,#3505,.T.);
#4881=ORIENTED_EDGE('',*,*,#3495,.F.);
#4882=ORIENTED_EDGE('',*,*,#3501,.F.);
#4883=ORIENTED_EDGE('',*,*,#3506,.T.);
#4884=ORIENTED_EDGE('',*,*,#3507,.T.);
#4885=ORIENTED_EDGE('',*,*,#3508,.T.);
#4886=ORIENTED_EDGE('',*,*,#3496,.F.);
#4887=ORIENTED_EDGE('',*,*,#3505,.F.);
#4888=ORIENTED_EDGE('',*,*,#3509,.T.);
#4889=ORIENTED_EDGE('',*,*,#3510,.T.);
#4890=ORIENTED_EDGE('',*,*,#3511,.T.);
#4891=ORIENTED_EDGE('',*,*,#3497,.F.);
#4892=ORIENTED_EDGE('',*,*,#3508,.F.);
#4893=ORIENTED_EDGE('',*,*,#3512,.T.);
#4894=ORIENTED_EDGE('',*,*,#3513,.T.);
#4895=ORIENTED_EDGE('',*,*,#3514,.T.);
#4896=ORIENTED_EDGE('',*,*,#3498,.F.);
#4897=ORIENTED_EDGE('',*,*,#3511,.F.);
#4898=ORIENTED_EDGE('',*,*,#3515,.T.);
#4899=ORIENTED_EDGE('',*,*,#3516,.T.);
#4900=ORIENTED_EDGE('',*,*,#3502,.T.);
#4901=ORIENTED_EDGE('',*,*,#3493,.F.);
#4902=ORIENTED_EDGE('',*,*,#3514,.F.);
#4903=ORIENTED_EDGE('',*,*,#3481,.F.);
#4904=ORIENTED_EDGE('',*,*,#3509,.F.);
#4905=ORIENTED_EDGE('',*,*,#3507,.F.);
#4906=ORIENTED_EDGE('',*,*,#3480,.F.);
#4907=ORIENTED_EDGE('',*,*,#3512,.F.);
#4908=ORIENTED_EDGE('',*,*,#3510,.F.);
#4909=ORIENTED_EDGE('',*,*,#3479,.F.);
#4910=ORIENTED_EDGE('',*,*,#3515,.F.);
#4911=ORIENTED_EDGE('',*,*,#3513,.F.);
#4912=ORIENTED_EDGE('',*,*,#3478,.F.);
#4913=ORIENTED_EDGE('',*,*,#3499,.F.);
#4914=ORIENTED_EDGE('',*,*,#3516,.F.);
#4915=ORIENTED_EDGE('',*,*,#3477,.F.);
#4916=ORIENTED_EDGE('',*,*,#3503,.F.);
#4917=ORIENTED_EDGE('',*,*,#3500,.F.);
#4918=ORIENTED_EDGE('',*,*,#3476,.F.);
#4919=ORIENTED_EDGE('',*,*,#3506,.F.);
#4920=ORIENTED_EDGE('',*,*,#3504,.F.);
#4921=ORIENTED_EDGE('',*,*,#3517,.T.);
#4922=ORIENTED_EDGE('',*,*,#3518,.T.);
#4923=ORIENTED_EDGE('',*,*,#3519,.T.);
#4924=ORIENTED_EDGE('',*,*,#3520,.T.);
#4925=ORIENTED_EDGE('',*,*,#3521,.T.);
#4926=ORIENTED_EDGE('',*,*,#3522,.T.);
#4927=ORIENTED_EDGE('',*,*,#3523,.T.);
#4928=ORIENTED_EDGE('',*,*,#3517,.F.);
#4929=ORIENTED_EDGE('',*,*,#3524,.F.);
#4930=ORIENTED_EDGE('',*,*,#3525,.T.);
#4931=ORIENTED_EDGE('',*,*,#3526,.F.);
#4932=ORIENTED_EDGE('',*,*,#3525,.F.);
#4933=ORIENTED_EDGE('',*,*,#3527,.F.);
#4934=ORIENTED_EDGE('',*,*,#3528,.T.);
#4935=ORIENTED_EDGE('',*,*,#3529,.T.);
#4936=ORIENTED_EDGE('',*,*,#3528,.F.);
#4937=ORIENTED_EDGE('',*,*,#3526,.T.);
#4938=ORIENTED_EDGE('',*,*,#3530,.T.);
#4939=ORIENTED_EDGE('',*,*,#3527,.T.);
#4940=ORIENTED_EDGE('',*,*,#3530,.F.);
#4941=ORIENTED_EDGE('',*,*,#3531,.F.);
#4942=ORIENTED_EDGE('',*,*,#3532,.T.);
#4943=ORIENTED_EDGE('',*,*,#3533,.T.);
#4944=ORIENTED_EDGE('',*,*,#3532,.F.);
#4945=ORIENTED_EDGE('',*,*,#3531,.T.);
#4946=ORIENTED_EDGE('',*,*,#3534,.F.);
#4947=ORIENTED_EDGE('',*,*,#3534,.T.);
#4948=ORIENTED_EDGE('',*,*,#3535,.T.);
#4949=ORIENTED_EDGE('',*,*,#3536,.T.);
#4950=ORIENTED_EDGE('',*,*,#3537,.T.);
#4951=ORIENTED_EDGE('',*,*,#3538,.T.);
#4952=ORIENTED_EDGE('',*,*,#3539,.T.);
#4953=ORIENTED_EDGE('',*,*,#3540,.T.);
#4954=ORIENTED_EDGE('',*,*,#3533,.F.);
#4955=ORIENTED_EDGE('',*,*,#3524,.T.);
#4956=ORIENTED_EDGE('',*,*,#3529,.F.);
#4957=ORIENTED_EDGE('',*,*,#3541,.T.);
#4958=ORIENTED_EDGE('',*,*,#3542,.T.);
#4959=ORIENTED_EDGE('',*,*,#3543,.T.);
#4960=ORIENTED_EDGE('',*,*,#3536,.F.);
#4961=ORIENTED_EDGE('',*,*,#3544,.F.);
#4962=ORIENTED_EDGE('',*,*,#3545,.T.);
#4963=ORIENTED_EDGE('',*,*,#3546,.T.);
#4964=ORIENTED_EDGE('',*,*,#3547,.T.);
#4965=ORIENTED_EDGE('',*,*,#3537,.F.);
#4966=ORIENTED_EDGE('',*,*,#3543,.F.);
#4967=ORIENTED_EDGE('',*,*,#3548,.T.);
#4968=ORIENTED_EDGE('',*,*,#3549,.T.);
#4969=ORIENTED_EDGE('',*,*,#3550,.T.);
#4970=ORIENTED_EDGE('',*,*,#3538,.F.);
#4971=ORIENTED_EDGE('',*,*,#3547,.F.);
#4972=ORIENTED_EDGE('',*,*,#3551,.T.);
#4973=ORIENTED_EDGE('',*,*,#3552,.T.);
#4974=ORIENTED_EDGE('',*,*,#3553,.T.);
#4975=ORIENTED_EDGE('',*,*,#3539,.F.);
#4976=ORIENTED_EDGE('',*,*,#3550,.F.);
#4977=ORIENTED_EDGE('',*,*,#3554,.T.);
#4978=ORIENTED_EDGE('',*,*,#3555,.T.);
#4979=ORIENTED_EDGE('',*,*,#3556,.T.);
#4980=ORIENTED_EDGE('',*,*,#3540,.F.);
#4981=ORIENTED_EDGE('',*,*,#3553,.F.);
#4982=ORIENTED_EDGE('',*,*,#3557,.T.);
#4983=ORIENTED_EDGE('',*,*,#3558,.T.);
#4984=ORIENTED_EDGE('',*,*,#3544,.T.);
#4985=ORIENTED_EDGE('',*,*,#3535,.F.);
#4986=ORIENTED_EDGE('',*,*,#3556,.F.);
#4987=ORIENTED_EDGE('',*,*,#3523,.F.);
#4988=ORIENTED_EDGE('',*,*,#3551,.F.);
#4989=ORIENTED_EDGE('',*,*,#3549,.F.);
#4990=ORIENTED_EDGE('',*,*,#3522,.F.);
#4991=ORIENTED_EDGE('',*,*,#3554,.F.);
#4992=ORIENTED_EDGE('',*,*,#3552,.F.);
#4993=ORIENTED_EDGE('',*,*,#3521,.F.);
#4994=ORIENTED_EDGE('',*,*,#3557,.F.);
#4995=ORIENTED_EDGE('',*,*,#3555,.F.);
#4996=ORIENTED_EDGE('',*,*,#3520,.F.);
#4997=ORIENTED_EDGE('',*,*,#3541,.F.);
#4998=ORIENTED_EDGE('',*,*,#3558,.F.);
#4999=ORIENTED_EDGE('',*,*,#3519,.F.);
#5000=ORIENTED_EDGE('',*,*,#3545,.F.);
#5001=ORIENTED_EDGE('',*,*,#3542,.F.);
#5002=ORIENTED_EDGE('',*,*,#3518,.F.);
#5003=ORIENTED_EDGE('',*,*,#3548,.F.);
#5004=ORIENTED_EDGE('',*,*,#3546,.F.);
#5005=ORIENTED_EDGE('',*,*,#3559,.T.);
#5006=ORIENTED_EDGE('',*,*,#3560,.T.);
#5007=ORIENTED_EDGE('',*,*,#3561,.T.);
#5008=ORIENTED_EDGE('',*,*,#3562,.T.);
#5009=ORIENTED_EDGE('',*,*,#3563,.T.);
#5010=ORIENTED_EDGE('',*,*,#3564,.T.);
#5011=ORIENTED_EDGE('',*,*,#3565,.T.);
#5012=ORIENTED_EDGE('',*,*,#3559,.F.);
#5013=ORIENTED_EDGE('',*,*,#3566,.F.);
#5014=ORIENTED_EDGE('',*,*,#3567,.T.);
#5015=ORIENTED_EDGE('',*,*,#3568,.F.);
#5016=ORIENTED_EDGE('',*,*,#3567,.F.);
#5017=ORIENTED_EDGE('',*,*,#3569,.F.);
#5018=ORIENTED_EDGE('',*,*,#3570,.T.);
#5019=ORIENTED_EDGE('',*,*,#3571,.T.);
#5020=ORIENTED_EDGE('',*,*,#3570,.F.);
#5021=ORIENTED_EDGE('',*,*,#3568,.T.);
#5022=ORIENTED_EDGE('',*,*,#3572,.T.);
#5023=ORIENTED_EDGE('',*,*,#3569,.T.);
#5024=ORIENTED_EDGE('',*,*,#3572,.F.);
#5025=ORIENTED_EDGE('',*,*,#3573,.F.);
#5026=ORIENTED_EDGE('',*,*,#3574,.T.);
#5027=ORIENTED_EDGE('',*,*,#3575,.T.);
#5028=ORIENTED_EDGE('',*,*,#3574,.F.);
#5029=ORIENTED_EDGE('',*,*,#3573,.T.);
#5030=ORIENTED_EDGE('',*,*,#3576,.F.);
#5031=ORIENTED_EDGE('',*,*,#3576,.T.);
#5032=ORIENTED_EDGE('',*,*,#3577,.T.);
#5033=ORIENTED_EDGE('',*,*,#3578,.T.);
#5034=ORIENTED_EDGE('',*,*,#3579,.T.);
#5035=ORIENTED_EDGE('',*,*,#3580,.T.);
#5036=ORIENTED_EDGE('',*,*,#3581,.T.);
#5037=ORIENTED_EDGE('',*,*,#3582,.T.);
#5038=ORIENTED_EDGE('',*,*,#3575,.F.);
#5039=ORIENTED_EDGE('',*,*,#3566,.T.);
#5040=ORIENTED_EDGE('',*,*,#3571,.F.);
#5041=ORIENTED_EDGE('',*,*,#3583,.T.);
#5042=ORIENTED_EDGE('',*,*,#3584,.T.);
#5043=ORIENTED_EDGE('',*,*,#3585,.T.);
#5044=ORIENTED_EDGE('',*,*,#3578,.F.);
#5045=ORIENTED_EDGE('',*,*,#3586,.F.);
#5046=ORIENTED_EDGE('',*,*,#3587,.T.);
#5047=ORIENTED_EDGE('',*,*,#3588,.T.);
#5048=ORIENTED_EDGE('',*,*,#3589,.T.);
#5049=ORIENTED_EDGE('',*,*,#3579,.F.);
#5050=ORIENTED_EDGE('',*,*,#3585,.F.);
#5051=ORIENTED_EDGE('',*,*,#3590,.T.);
#5052=ORIENTED_EDGE('',*,*,#3591,.T.);
#5053=ORIENTED_EDGE('',*,*,#3592,.T.);
#5054=ORIENTED_EDGE('',*,*,#3580,.F.);
#5055=ORIENTED_EDGE('',*,*,#3589,.F.);
#5056=ORIENTED_EDGE('',*,*,#3593,.T.);
#5057=ORIENTED_EDGE('',*,*,#3594,.T.);
#5058=ORIENTED_EDGE('',*,*,#3595,.T.);
#5059=ORIENTED_EDGE('',*,*,#3581,.F.);
#5060=ORIENTED_EDGE('',*,*,#3592,.F.);
#5061=ORIENTED_EDGE('',*,*,#3596,.T.);
#5062=ORIENTED_EDGE('',*,*,#3597,.T.);
#5063=ORIENTED_EDGE('',*,*,#3598,.T.);
#5064=ORIENTED_EDGE('',*,*,#3582,.F.);
#5065=ORIENTED_EDGE('',*,*,#3595,.F.);
#5066=ORIENTED_EDGE('',*,*,#3599,.T.);
#5067=ORIENTED_EDGE('',*,*,#3600,.T.);
#5068=ORIENTED_EDGE('',*,*,#3586,.T.);
#5069=ORIENTED_EDGE('',*,*,#3577,.F.);
#5070=ORIENTED_EDGE('',*,*,#3598,.F.);
#5071=ORIENTED_EDGE('',*,*,#3565,.F.);
#5072=ORIENTED_EDGE('',*,*,#3593,.F.);
#5073=ORIENTED_EDGE('',*,*,#3591,.F.);
#5074=ORIENTED_EDGE('',*,*,#3564,.F.);
#5075=ORIENTED_EDGE('',*,*,#3596,.F.);
#5076=ORIENTED_EDGE('',*,*,#3594,.F.);
#5077=ORIENTED_EDGE('',*,*,#3563,.F.);
#5078=ORIENTED_EDGE('',*,*,#3599,.F.);
#5079=ORIENTED_EDGE('',*,*,#3597,.F.);
#5080=ORIENTED_EDGE('',*,*,#3562,.F.);
#5081=ORIENTED_EDGE('',*,*,#3583,.F.);
#5082=ORIENTED_EDGE('',*,*,#3600,.F.);
#5083=ORIENTED_EDGE('',*,*,#3561,.F.);
#5084=ORIENTED_EDGE('',*,*,#3587,.F.);
#5085=ORIENTED_EDGE('',*,*,#3584,.F.);
#5086=ORIENTED_EDGE('',*,*,#3560,.F.);
#5087=ORIENTED_EDGE('',*,*,#3590,.F.);
#5088=ORIENTED_EDGE('',*,*,#3588,.F.);
#5089=ORIENTED_EDGE('',*,*,#3601,.T.);
#5090=ORIENTED_EDGE('',*,*,#3602,.T.);
#5091=ORIENTED_EDGE('',*,*,#3603,.T.);
#5092=ORIENTED_EDGE('',*,*,#3604,.T.);
#5093=ORIENTED_EDGE('',*,*,#3605,.T.);
#5094=ORIENTED_EDGE('',*,*,#3606,.T.);
#5095=ORIENTED_EDGE('',*,*,#3607,.T.);
#5096=ORIENTED_EDGE('',*,*,#3601,.F.);
#5097=ORIENTED_EDGE('',*,*,#3608,.F.);
#5098=ORIENTED_EDGE('',*,*,#3609,.T.);
#5099=ORIENTED_EDGE('',*,*,#3610,.F.);
#5100=ORIENTED_EDGE('',*,*,#3609,.F.);
#5101=ORIENTED_EDGE('',*,*,#3611,.F.);
#5102=ORIENTED_EDGE('',*,*,#3612,.T.);
#5103=ORIENTED_EDGE('',*,*,#3613,.T.);
#5104=ORIENTED_EDGE('',*,*,#3612,.F.);
#5105=ORIENTED_EDGE('',*,*,#3610,.T.);
#5106=ORIENTED_EDGE('',*,*,#3614,.T.);
#5107=ORIENTED_EDGE('',*,*,#3611,.T.);
#5108=ORIENTED_EDGE('',*,*,#3614,.F.);
#5109=ORIENTED_EDGE('',*,*,#3615,.F.);
#5110=ORIENTED_EDGE('',*,*,#3616,.T.);
#5111=ORIENTED_EDGE('',*,*,#3617,.T.);
#5112=ORIENTED_EDGE('',*,*,#3616,.F.);
#5113=ORIENTED_EDGE('',*,*,#3615,.T.);
#5114=ORIENTED_EDGE('',*,*,#3618,.F.);
#5115=ORIENTED_EDGE('',*,*,#3618,.T.);
#5116=ORIENTED_EDGE('',*,*,#3619,.T.);
#5117=ORIENTED_EDGE('',*,*,#3620,.T.);
#5118=ORIENTED_EDGE('',*,*,#3621,.T.);
#5119=ORIENTED_EDGE('',*,*,#3622,.T.);
#5120=ORIENTED_EDGE('',*,*,#3623,.T.);
#5121=ORIENTED_EDGE('',*,*,#3624,.T.);
#5122=ORIENTED_EDGE('',*,*,#3617,.F.);
#5123=ORIENTED_EDGE('',*,*,#3608,.T.);
#5124=ORIENTED_EDGE('',*,*,#3613,.F.);
#5125=ORIENTED_EDGE('',*,*,#3625,.T.);
#5126=ORIENTED_EDGE('',*,*,#3626,.T.);
#5127=ORIENTED_EDGE('',*,*,#3627,.T.);
#5128=ORIENTED_EDGE('',*,*,#3620,.F.);
#5129=ORIENTED_EDGE('',*,*,#3628,.F.);
#5130=ORIENTED_EDGE('',*,*,#3629,.T.);
#5131=ORIENTED_EDGE('',*,*,#3630,.T.);
#5132=ORIENTED_EDGE('',*,*,#3631,.T.);
#5133=ORIENTED_EDGE('',*,*,#3621,.F.);
#5134=ORIENTED_EDGE('',*,*,#3627,.F.);
#5135=ORIENTED_EDGE('',*,*,#3632,.T.);
#5136=ORIENTED_EDGE('',*,*,#3633,.T.);
#5137=ORIENTED_EDGE('',*,*,#3634,.T.);
#5138=ORIENTED_EDGE('',*,*,#3622,.F.);
#5139=ORIENTED_EDGE('',*,*,#3631,.F.);
#5140=ORIENTED_EDGE('',*,*,#3635,.T.);
#5141=ORIENTED_EDGE('',*,*,#3636,.T.);
#5142=ORIENTED_EDGE('',*,*,#3637,.T.);
#5143=ORIENTED_EDGE('',*,*,#3623,.F.);
#5144=ORIENTED_EDGE('',*,*,#3634,.F.);
#5145=ORIENTED_EDGE('',*,*,#3638,.T.);
#5146=ORIENTED_EDGE('',*,*,#3639,.T.);
#5147=ORIENTED_EDGE('',*,*,#3640,.T.);
#5148=ORIENTED_EDGE('',*,*,#3624,.F.);
#5149=ORIENTED_EDGE('',*,*,#3637,.F.);
#5150=ORIENTED_EDGE('',*,*,#3641,.T.);
#5151=ORIENTED_EDGE('',*,*,#3642,.T.);
#5152=ORIENTED_EDGE('',*,*,#3628,.T.);
#5153=ORIENTED_EDGE('',*,*,#3619,.F.);
#5154=ORIENTED_EDGE('',*,*,#3640,.F.);
#5155=ORIENTED_EDGE('',*,*,#3607,.F.);
#5156=ORIENTED_EDGE('',*,*,#3635,.F.);
#5157=ORIENTED_EDGE('',*,*,#3633,.F.);
#5158=ORIENTED_EDGE('',*,*,#3606,.F.);
#5159=ORIENTED_EDGE('',*,*,#3638,.F.);
#5160=ORIENTED_EDGE('',*,*,#3636,.F.);
#5161=ORIENTED_EDGE('',*,*,#3605,.F.);
#5162=ORIENTED_EDGE('',*,*,#3641,.F.);
#5163=ORIENTED_EDGE('',*,*,#3639,.F.);
#5164=ORIENTED_EDGE('',*,*,#3604,.F.);
#5165=ORIENTED_EDGE('',*,*,#3625,.F.);
#5166=ORIENTED_EDGE('',*,*,#3642,.F.);
#5167=ORIENTED_EDGE('',*,*,#3603,.F.);
#5168=ORIENTED_EDGE('',*,*,#3629,.F.);
#5169=ORIENTED_EDGE('',*,*,#3626,.F.);
#5170=ORIENTED_EDGE('',*,*,#3602,.F.);
#5171=ORIENTED_EDGE('',*,*,#3632,.F.);
#5172=ORIENTED_EDGE('',*,*,#3630,.F.);
#5173=CYLINDRICAL_SURFACE('',#5681,1.99999999999998);
#5174=CYLINDRICAL_SURFACE('',#5684,1.99999999999998);
#5175=CYLINDRICAL_SURFACE('',#5687,2.);
#5176=CYLINDRICAL_SURFACE('',#5690,2.5);
#5177=CYLINDRICAL_SURFACE('',#5693,2.5);
#5178=CYLINDRICAL_SURFACE('',#5696,2.5);
#5179=CYLINDRICAL_SURFACE('',#5699,2.5);
#5180=CYLINDRICAL_SURFACE('',#5702,8.00000000000001);
#5181=CYLINDRICAL_SURFACE('',#5706,8.);
#5182=CYLINDRICAL_SURFACE('',#5710,8.);
#5183=CYLINDRICAL_SURFACE('',#5714,8.);
#5184=CYLINDRICAL_SURFACE('',#5720,1.99999999999998);
#5185=CYLINDRICAL_SURFACE('',#5723,1.99999999999998);
#5186=CYLINDRICAL_SURFACE('',#5726,2.5);
#5187=CYLINDRICAL_SURFACE('',#5729,2.5);
#5188=CYLINDRICAL_SURFACE('',#5732,8.00000000000001);
#5189=CYLINDRICAL_SURFACE('',#5735,2.5);
#5190=CYLINDRICAL_SURFACE('',#5738,2.5);
#5191=CYLINDRICAL_SURFACE('',#5741,2.);
#5192=CYLINDRICAL_SURFACE('',#5745,8.);
#5193=CYLINDRICAL_SURFACE('',#5749,8.);
#5194=CYLINDRICAL_SURFACE('',#5753,8.);
#5195=CYLINDRICAL_SURFACE('',#5784,3.5);
#5196=CYLINDRICAL_SURFACE('',#5787,4.5);
#5197=CYLINDRICAL_SURFACE('',#5790,3.5);
#5198=CYLINDRICAL_SURFACE('',#5793,2.5);
#5199=CYLINDRICAL_SURFACE('',#5796,2.5);
#5200=CYLINDRICAL_SURFACE('',#5818,6.50000000000001);
#5201=CYLINDRICAL_SURFACE('',#5820,10.);
#5202=CYLINDRICAL_SURFACE('',#5827,23.);
#5203=CYLINDRICAL_SURFACE('',#5840,24.9999999999999);
#5204=CYLINDRICAL_SURFACE('',#5846,24.9999999999999);
#5205=CYLINDRICAL_SURFACE('',#5850,4.5);
#5206=CYLINDRICAL_SURFACE('',#5856,12.);
#5207=CYLINDRICAL_SURFACE('',#5863,12.);
#5208=CYLINDRICAL_SURFACE('',#5872,24.9999999999999);
#5209=CYLINDRICAL_SURFACE('',#5880,24.9999999999999);
#5210=CYLINDRICAL_SURFACE('',#5885,7.);
#5211=CYLINDRICAL_SURFACE('',#5888,14.);
#5212=CYLINDRICAL_SURFACE('',#5891,7.);
#5213=CYLINDRICAL_SURFACE('',#5894,14.);
#5214=CYLINDRICAL_SURFACE('',#5897,2.5);
#5215=CYLINDRICAL_SURFACE('',#5900,16.25);
#5216=CYLINDRICAL_SURFACE('',#5985,19.);
#5217=CYLINDRICAL_SURFACE('',#5986,16.25);
#5218=CYLINDRICAL_SURFACE('',#5987,19.);
#5219=CYLINDRICAL_SURFACE('',#5988,16.25);
#5220=CYLINDRICAL_SURFACE('',#5989,19.);
#5221=CYLINDRICAL_SURFACE('',#5990,16.25);
#5222=CYLINDRICAL_SURFACE('',#5991,19.);
#5223=CYLINDRICAL_SURFACE('',#5992,16.25);
#5224=CYLINDRICAL_SURFACE('',#5993,19.);
#5225=CYLINDRICAL_SURFACE('',#5994,16.25);
#5226=CYLINDRICAL_SURFACE('',#5995,19.);
#5227=CYLINDRICAL_SURFACE('',#5996,16.25);
#5228=CYLINDRICAL_SURFACE('',#5997,19.);
#5229=CYLINDRICAL_SURFACE('',#5998,16.25);
#5230=CYLINDRICAL_SURFACE('',#5999,19.);
#5231=CYLINDRICAL_SURFACE('',#6000,16.25);
#5232=CYLINDRICAL_SURFACE('',#6001,19.);
#5233=CYLINDRICAL_SURFACE('',#6002,19.);
#5234=CYLINDRICAL_SURFACE('',#6003,16.25);
#5235=CYLINDRICAL_SURFACE('',#6004,19.);
#5236=CYLINDRICAL_SURFACE('',#6005,16.25);
#5237=CYLINDRICAL_SURFACE('',#6006,19.);
#5238=CYLINDRICAL_SURFACE('',#6007,16.25);
#5239=CYLINDRICAL_SURFACE('',#6008,19.);
#5240=CYLINDRICAL_SURFACE('',#6009,16.25);
#5241=CYLINDRICAL_SURFACE('',#6010,19.);
#5242=CYLINDRICAL_SURFACE('',#6011,16.25);
#5243=CYLINDRICAL_SURFACE('',#6012,19.);
#5244=CYLINDRICAL_SURFACE('',#6013,16.25);
#5245=CYLINDRICAL_SURFACE('',#6014,19.);
#5246=CYLINDRICAL_SURFACE('',#6015,16.25);
#5247=CYLINDRICAL_SURFACE('',#6016,19.);
#5248=CYLINDRICAL_SURFACE('',#6017,16.25);
#5249=CYLINDRICAL_SURFACE('',#6018,19.);
#5250=CYLINDRICAL_SURFACE('',#6019,16.25);
#5251=CYLINDRICAL_SURFACE('',#6020,19.);
#5252=CYLINDRICAL_SURFACE('',#6021,16.25);
#5253=CYLINDRICAL_SURFACE('',#6022,19.);
#5254=CYLINDRICAL_SURFACE('',#6023,16.25);
#5255=CYLINDRICAL_SURFACE('',#6027,2.5);
#5256=CYLINDRICAL_SURFACE('',#6030,2.5);
#5257=CYLINDRICAL_SURFACE('',#6039,5.);
#5258=CYLINDRICAL_SURFACE('',#6041,5.);
#5259=CYLINDRICAL_SURFACE('',#6058,2.);
#5260=CYLINDRICAL_SURFACE('',#6059,3.8);
#5261=CYLINDRICAL_SURFACE('',#6094,2.);
#5262=CYLINDRICAL_SURFACE('',#6095,3.8);
#5263=CYLINDRICAL_SURFACE('',#6130,2.);
#5264=CYLINDRICAL_SURFACE('',#6131,3.8);
#5265=CYLINDRICAL_SURFACE('',#6166,1.5);
#5266=CYLINDRICAL_SURFACE('',#6167,2.85);
#5267=ADVANCED_FACE('',(#550),#5173,.F.);
#5268=ADVANCED_FACE('',(#551),#5174,.F.);
#5269=ADVANCED_FACE('',(#552),#5175,.F.);
#5270=ADVANCED_FACE('',(#553),#5176,.F.);
#5271=ADVANCED_FACE('',(#554),#5177,.F.);
#5272=ADVANCED_FACE('',(#555),#5178,.F.);
#5273=ADVANCED_FACE('',(#556),#5179,.F.);
#5274=ADVANCED_FACE('',(#557),#5180,.T.);
#5275=ADVANCED_FACE('',(#558),#389,.F.);
#5276=ADVANCED_FACE('',(#559),#5181,.T.);
#5277=ADVANCED_FACE('',(#560),#390,.F.);
#5278=ADVANCED_FACE('',(#561),#5182,.T.);
#5279=ADVANCED_FACE('',(#562),#391,.F.);
#5280=ADVANCED_FACE('',(#563),#5183,.T.);
#5281=ADVANCED_FACE('',(#564),#392,.F.);
#5282=ADVANCED_FACE('',(#565,#327,#328,#329,#330,#331,#332,#333),#393,.T.);
#5283=ADVANCED_FACE('',(#566,#334,#335,#336,#337,#338,#339,#340),#394,.F.);
#5284=ADVANCED_FACE('',(#567),#5184,.F.);
#5285=ADVANCED_FACE('',(#568),#5185,.F.);
#5286=ADVANCED_FACE('',(#569),#5186,.F.);
#5287=ADVANCED_FACE('',(#570),#5187,.F.);
#5288=ADVANCED_FACE('',(#571),#5188,.T.);
#5289=ADVANCED_FACE('',(#572),#5189,.F.);
#5290=ADVANCED_FACE('',(#573),#5190,.F.);
#5291=ADVANCED_FACE('',(#574),#5191,.F.);
#5292=ADVANCED_FACE('',(#575),#395,.F.);
#5293=ADVANCED_FACE('',(#576),#5192,.T.);
#5294=ADVANCED_FACE('',(#577),#396,.F.);
#5295=ADVANCED_FACE('',(#578),#5193,.T.);
#5296=ADVANCED_FACE('',(#579),#397,.F.);
#5297=ADVANCED_FACE('',(#580),#5194,.T.);
#5298=ADVANCED_FACE('',(#581),#398,.F.);
#5299=ADVANCED_FACE('',(#582,#341,#342,#343,#344,#345,#346,#347),#399,.F.);
#5300=ADVANCED_FACE('',(#583,#348,#349,#350,#351,#352,#353,#354),#400,.F.);
#5301=ADVANCED_FACE('',(#584),#401,.F.);
#5302=ADVANCED_FACE('',(#585),#402,.F.);
#5303=ADVANCED_FACE('',(#586),#403,.F.);
#5304=ADVANCED_FACE('',(#587),#404,.F.);
#5305=ADVANCED_FACE('',(#588),#405,.F.);
#5306=ADVANCED_FACE('',(#589),#406,.F.);
#5307=ADVANCED_FACE('',(#590),#407,.T.);
#5308=ADVANCED_FACE('',(#591),#408,.F.);
#5309=ADVANCED_FACE('',(#592),#409,.F.);
#5310=ADVANCED_FACE('',(#593),#410,.F.);
#5311=ADVANCED_FACE('',(#594),#411,.F.);
#5312=ADVANCED_FACE('',(#595),#412,.F.);
#5313=ADVANCED_FACE('',(#596),#413,.F.);
#5314=ADVANCED_FACE('',(#597),#414,.F.);
#5315=ADVANCED_FACE('',(#598),#415,.T.);
#5316=ADVANCED_FACE('',(#599),#416,.F.);
#5317=ADVANCED_FACE('',(#600),#417,.F.);
#5318=ADVANCED_FACE('',(#601),#418,.F.);
#5319=ADVANCED_FACE('',(#602),#419,.F.);
#5320=ADVANCED_FACE('',(#603),#420,.F.);
#5321=ADVANCED_FACE('',(#604),#421,.F.);
#5322=ADVANCED_FACE('',(#605),#422,.F.);
#5323=ADVANCED_FACE('',(#606),#423,.T.);
#5324=ADVANCED_FACE('',(#607),#424,.F.);
#5325=ADVANCED_FACE('',(#608),#5195,.T.);
#5326=ADVANCED_FACE('',(#609),#5196,.T.);
#5327=ADVANCED_FACE('',(#610),#5197,.T.);
#5328=ADVANCED_FACE('',(#611),#5198,.F.);
#5329=ADVANCED_FACE('',(#612),#5199,.F.);
#5330=ADVANCED_FACE('',(#613,#355),#425,.F.);
#5331=ADVANCED_FACE('',(#614,#356),#426,.T.);
#5332=ADVANCED_FACE('',(#615,#357,#358,#359,#360),#427,.T.);
#5333=ADVANCED_FACE('',(#616,#361,#362,#363,#364),#428,.F.);
#5334=ADVANCED_FACE('',(#617),#429,.F.);
#5335=ADVANCED_FACE('',(#618),#430,.F.);
#5336=ADVANCED_FACE('',(#619),#5200,.T.);
#5337=ADVANCED_FACE('',(#620),#431,.F.);
#5338=ADVANCED_FACE('',(#621),#5201,.F.);
#5339=ADVANCED_FACE('',(#622),#432,.F.);
#5340=ADVANCED_FACE('',(#623),#433,.F.);
#5341=ADVANCED_FACE('',(#624),#434,.F.);
#5342=ADVANCED_FACE('',(#625),#435,.F.);
#5343=ADVANCED_FACE('',(#626),#436,.F.);
#5344=ADVANCED_FACE('',(#627),#437,.F.);
#5345=ADVANCED_FACE('',(#628),#5202,.F.);
#5346=ADVANCED_FACE('',(#629),#438,.F.);
#5347=ADVANCED_FACE('',(#630),#439,.F.);
#5348=ADVANCED_FACE('',(#631),#440,.F.);
#5349=ADVANCED_FACE('',(#632),#441,.F.);
#5350=ADVANCED_FACE('',(#633),#442,.F.);
#5351=ADVANCED_FACE('',(#634),#443,.F.);
#5352=ADVANCED_FACE('',(#635),#444,.F.);
#5353=ADVANCED_FACE('',(#636),#445,.F.);
#5354=ADVANCED_FACE('',(#637),#446,.F.);
#5355=ADVANCED_FACE('',(#638),#447,.F.);
#5356=ADVANCED_FACE('',(#639),#448,.F.);
#5357=ADVANCED_FACE('',(#640),#449,.F.);
#5358=ADVANCED_FACE('',(#641),#5203,.T.);
#5359=ADVANCED_FACE('',(#642),#450,.T.);
#5360=ADVANCED_FACE('',(#643),#451,.F.);
#5361=ADVANCED_FACE('',(#644),#452,.F.);
#5362=ADVANCED_FACE('',(#645),#453,.F.);
#5363=ADVANCED_FACE('',(#646),#5204,.T.);
#5364=ADVANCED_FACE('',(#647),#454,.F.);
#5365=ADVANCED_FACE('',(#648),#455,.T.);
#5366=ADVANCED_FACE('',(#649),#5205,.T.);
#5367=ADVANCED_FACE('',(#650),#456,.F.);
#5368=ADVANCED_FACE('',(#651),#457,.F.);
#5369=ADVANCED_FACE('',(#652),#458,.F.);
#5370=ADVANCED_FACE('',(#653),#459,.F.);
#5371=ADVANCED_FACE('',(#654),#5206,.T.);
#5372=ADVANCED_FACE('',(#655),#460,.F.);
#5373=ADVANCED_FACE('',(#656),#461,.F.);
#5374=ADVANCED_FACE('',(#657,#365),#462,.T.);
#5375=ADVANCED_FACE('',(#658),#463,.F.);
#5376=ADVANCED_FACE('',(#659),#464,.F.);
#5377=ADVANCED_FACE('',(#660),#5207,.T.);
#5378=ADVANCED_FACE('',(#661),#465,.F.);
#5379=ADVANCED_FACE('',(#662),#466,.F.);
#5380=ADVANCED_FACE('',(#663),#467,.F.);
#5381=ADVANCED_FACE('',(#664),#468,.F.);
#5382=ADVANCED_FACE('',(#665,#366),#469,.T.);
#5383=ADVANCED_FACE('',(#666),#470,.F.);
#5384=ADVANCED_FACE('',(#667),#471,.F.);
#5385=ADVANCED_FACE('',(#668),#5208,.T.);
#5386=ADVANCED_FACE('',(#669),#472,.F.);
#5387=ADVANCED_FACE('',(#670),#473,.F.);
#5388=ADVANCED_FACE('',(#671),#474,.T.);
#5389=ADVANCED_FACE('',(#672),#475,.F.);
#5390=ADVANCED_FACE('',(#673),#476,.F.);
#5391=ADVANCED_FACE('',(#674),#477,.F.);
#5392=ADVANCED_FACE('',(#675),#5209,.T.);
#5393=ADVANCED_FACE('',(#676),#478,.F.);
#5394=ADVANCED_FACE('',(#677),#479,.T.);
#5395=ADVANCED_FACE('',(#678),#5210,.T.);
#5396=ADVANCED_FACE('',(#679),#5211,.F.);
#5397=ADVANCED_FACE('',(#680),#5212,.T.);
#5398=ADVANCED_FACE('',(#681),#5213,.F.);
#5399=ADVANCED_FACE('',(#682),#5214,.F.);
#5400=ADVANCED_FACE('',(#683),#5215,.T.);
#5401=ADVANCED_FACE('',(#684,#367),#480,.F.);
#5402=ADVANCED_FACE('',(#685,#368),#481,.T.);
#5403=ADVANCED_FACE('',(#686,#369),#482,.T.);
#5404=ADVANCED_FACE('',(#687,#370),#483,.F.);
#5405=ADVANCED_FACE('',(#688),#167,.F.);
#5406=ADVANCED_FACE('',(#689),#5216,.T.);
#5407=ADVANCED_FACE('',(#690),#168,.F.);
#5408=ADVANCED_FACE('',(#691),#5217,.T.);
#5409=ADVANCED_FACE('',(#692),#169,.F.);
#5410=ADVANCED_FACE('',(#693),#5218,.T.);
#5411=ADVANCED_FACE('',(#694),#170,.F.);
#5412=ADVANCED_FACE('',(#695),#5219,.T.);
#5413=ADVANCED_FACE('',(#696),#171,.F.);
#5414=ADVANCED_FACE('',(#697),#5220,.T.);
#5415=ADVANCED_FACE('',(#698),#172,.F.);
#5416=ADVANCED_FACE('',(#699),#5221,.T.);
#5417=ADVANCED_FACE('',(#700),#173,.F.);
#5418=ADVANCED_FACE('',(#701),#5222,.T.);
#5419=ADVANCED_FACE('',(#702),#174,.F.);
#5420=ADVANCED_FACE('',(#703),#5223,.T.);
#5421=ADVANCED_FACE('',(#704),#175,.F.);
#5422=ADVANCED_FACE('',(#705),#5224,.T.);
#5423=ADVANCED_FACE('',(#706),#176,.F.);
#5424=ADVANCED_FACE('',(#707),#5225,.T.);
#5425=ADVANCED_FACE('',(#708),#177,.F.);
#5426=ADVANCED_FACE('',(#709),#5226,.T.);
#5427=ADVANCED_FACE('',(#710),#178,.F.);
#5428=ADVANCED_FACE('',(#711),#5227,.T.);
#5429=ADVANCED_FACE('',(#712),#179,.F.);
#5430=ADVANCED_FACE('',(#713),#5228,.T.);
#5431=ADVANCED_FACE('',(#714),#180,.F.);
#5432=ADVANCED_FACE('',(#715),#5229,.T.);
#5433=ADVANCED_FACE('',(#716),#181,.F.);
#5434=ADVANCED_FACE('',(#717),#5230,.T.);
#5435=ADVANCED_FACE('',(#718),#182,.F.);
#5436=ADVANCED_FACE('',(#719),#5231,.T.);
#5437=ADVANCED_FACE('',(#720),#183,.F.);
#5438=ADVANCED_FACE('',(#721),#5232,.T.);
#5439=ADVANCED_FACE('',(#722),#184,.F.);
#5440=ADVANCED_FACE('',(#723),#185,.F.);
#5441=ADVANCED_FACE('',(#724),#5233,.T.);
#5442=ADVANCED_FACE('',(#725),#186,.F.);
#5443=ADVANCED_FACE('',(#726),#5234,.T.);
#5444=ADVANCED_FACE('',(#727),#187,.F.);
#5445=ADVANCED_FACE('',(#728),#5235,.T.);
#5446=ADVANCED_FACE('',(#729),#188,.F.);
#5447=ADVANCED_FACE('',(#730),#5236,.T.);
#5448=ADVANCED_FACE('',(#731),#189,.F.);
#5449=ADVANCED_FACE('',(#732),#5237,.T.);
#5450=ADVANCED_FACE('',(#733),#190,.F.);
#5451=ADVANCED_FACE('',(#734),#5238,.T.);
#5452=ADVANCED_FACE('',(#735),#191,.F.);
#5453=ADVANCED_FACE('',(#736),#5239,.T.);
#5454=ADVANCED_FACE('',(#737),#192,.F.);
#5455=ADVANCED_FACE('',(#738),#5240,.T.);
#5456=ADVANCED_FACE('',(#739),#193,.F.);
#5457=ADVANCED_FACE('',(#740),#5241,.T.);
#5458=ADVANCED_FACE('',(#741),#194,.F.);
#5459=ADVANCED_FACE('',(#742),#5242,.T.);
#5460=ADVANCED_FACE('',(#743),#195,.F.);
#5461=ADVANCED_FACE('',(#744),#5243,.T.);
#5462=ADVANCED_FACE('',(#745),#196,.F.);
#5463=ADVANCED_FACE('',(#746),#5244,.T.);
#5464=ADVANCED_FACE('',(#747),#197,.F.);
#5465=ADVANCED_FACE('',(#748),#5245,.T.);
#5466=ADVANCED_FACE('',(#749),#198,.F.);
#5467=ADVANCED_FACE('',(#750),#5246,.T.);
#5468=ADVANCED_FACE('',(#751),#199,.F.);
#5469=ADVANCED_FACE('',(#752),#5247,.T.);
#5470=ADVANCED_FACE('',(#753),#200,.F.);
#5471=ADVANCED_FACE('',(#754),#5248,.T.);
#5472=ADVANCED_FACE('',(#755),#201,.F.);
#5473=ADVANCED_FACE('',(#756),#5249,.T.);
#5474=ADVANCED_FACE('',(#757),#202,.F.);
#5475=ADVANCED_FACE('',(#758),#5250,.T.);
#5476=ADVANCED_FACE('',(#759),#203,.F.);
#5477=ADVANCED_FACE('',(#760),#5251,.T.);
#5478=ADVANCED_FACE('',(#761),#204,.F.);
#5479=ADVANCED_FACE('',(#762),#5252,.T.);
#5480=ADVANCED_FACE('',(#763),#205,.F.);
#5481=ADVANCED_FACE('',(#764),#5253,.T.);
#5482=ADVANCED_FACE('',(#765),#206,.F.);
#5483=ADVANCED_FACE('',(#766),#5254,.T.);
#5484=ADVANCED_FACE('',(#767,#371),#484,.T.);
#5485=ADVANCED_FACE('',(#768,#372),#485,.T.);
#5486=ADVANCED_FACE('',(#769),#5255,.F.);
#5487=ADVANCED_FACE('',(#770),#5256,.F.);
#5488=ADVANCED_FACE('',(#771,#373,#374),#486,.T.);
#5489=ADVANCED_FACE('',(#772,#375,#376),#487,.F.);
#5490=ADVANCED_FACE('',(#773),#5257,.T.);
#5491=ADVANCED_FACE('',(#774),#488,.F.);
#5492=ADVANCED_FACE('',(#775),#5258,.T.);
#5493=ADVANCED_FACE('',(#776),#489,.F.);
#5494=ADVANCED_FACE('',(#777),#159,.F.);
#5495=ADVANCED_FACE('',(#778),#155,.F.);
#5496=ADVANCED_FACE('',(#779),#160,.T.);
#5497=ADVANCED_FACE('',(#780),#5259,.T.);
#5498=ADVANCED_FACE('',(#781),#5260,.T.);
#5499=ADVANCED_FACE('',(#782,#377),#151,.T.);
#5500=ADVANCED_FACE('',(#783,#378),#490,.T.);
#5501=ADVANCED_FACE('',(#784,#379),#491,.F.);
#5502=ADVANCED_FACE('',(#785),#492,.F.);
#5503=ADVANCED_FACE('',(#786),#493,.T.);
#5504=ADVANCED_FACE('',(#787),#494,.T.);
#5505=ADVANCED_FACE('',(#788),#495,.T.);
#5506=ADVANCED_FACE('',(#789),#496,.T.);
#5507=ADVANCED_FACE('',(#790),#497,.T.);
#5508=ADVANCED_FACE('',(#791),#498,.T.);
#5509=ADVANCED_FACE('',(#792),#499,.F.);
#5510=ADVANCED_FACE('',(#793),#500,.F.);
#5511=ADVANCED_FACE('',(#794),#501,.F.);
#5512=ADVANCED_FACE('',(#795),#502,.F.);
#5513=ADVANCED_FACE('',(#796),#503,.F.);
#5514=ADVANCED_FACE('',(#797),#504,.F.);
#5515=ADVANCED_FACE('',(#798),#161,.F.);
#5516=ADVANCED_FACE('',(#799),#156,.F.);
#5517=ADVANCED_FACE('',(#800),#162,.T.);
#5518=ADVANCED_FACE('',(#801),#5261,.T.);
#5519=ADVANCED_FACE('',(#802),#5262,.T.);
#5520=ADVANCED_FACE('',(#803,#380),#152,.T.);
#5521=ADVANCED_FACE('',(#804,#381),#505,.T.);
#5522=ADVANCED_FACE('',(#805,#382),#506,.F.);
#5523=ADVANCED_FACE('',(#806),#507,.F.);
#5524=ADVANCED_FACE('',(#807),#508,.T.);
#5525=ADVANCED_FACE('',(#808),#509,.T.);
#5526=ADVANCED_FACE('',(#809),#510,.T.);
#5527=ADVANCED_FACE('',(#810),#511,.T.);
#5528=ADVANCED_FACE('',(#811),#512,.T.);
#5529=ADVANCED_FACE('',(#812),#513,.T.);
#5530=ADVANCED_FACE('',(#813),#514,.F.);
#5531=ADVANCED_FACE('',(#814),#515,.F.);
#5532=ADVANCED_FACE('',(#815),#516,.F.);
#5533=ADVANCED_FACE('',(#816),#517,.F.);
#5534=ADVANCED_FACE('',(#817),#518,.F.);
#5535=ADVANCED_FACE('',(#818),#519,.F.);
#5536=ADVANCED_FACE('',(#819),#163,.F.);
#5537=ADVANCED_FACE('',(#820),#157,.F.);
#5538=ADVANCED_FACE('',(#821),#164,.T.);
#5539=ADVANCED_FACE('',(#822),#5263,.T.);
#5540=ADVANCED_FACE('',(#823),#5264,.T.);
#5541=ADVANCED_FACE('',(#824,#383),#153,.T.);
#5542=ADVANCED_FACE('',(#825,#384),#520,.T.);
#5543=ADVANCED_FACE('',(#826,#385),#521,.F.);
#5544=ADVANCED_FACE('',(#827),#522,.F.);
#5545=ADVANCED_FACE('',(#828),#523,.T.);
#5546=ADVANCED_FACE('',(#829),#524,.T.);
#5547=ADVANCED_FACE('',(#830),#525,.T.);
#5548=ADVANCED_FACE('',(#831),#526,.T.);
#5549=ADVANCED_FACE('',(#832),#527,.T.);
#5550=ADVANCED_FACE('',(#833),#528,.T.);
#5551=ADVANCED_FACE('',(#834),#529,.F.);
#5552=ADVANCED_FACE('',(#835),#530,.F.);
#5553=ADVANCED_FACE('',(#836),#531,.F.);
#5554=ADVANCED_FACE('',(#837),#532,.F.);
#5555=ADVANCED_FACE('',(#838),#533,.F.);
#5556=ADVANCED_FACE('',(#839),#534,.F.);
#5557=ADVANCED_FACE('',(#840),#165,.F.);
#5558=ADVANCED_FACE('',(#841),#158,.F.);
#5559=ADVANCED_FACE('',(#842),#166,.T.);
#5560=ADVANCED_FACE('',(#843),#5265,.T.);
#5561=ADVANCED_FACE('',(#844),#5266,.T.);
#5562=ADVANCED_FACE('',(#845,#386),#154,.T.);
#5563=ADVANCED_FACE('',(#846,#387),#535,.T.);
#5564=ADVANCED_FACE('',(#847,#388),#536,.F.);
#5565=ADVANCED_FACE('',(#848),#537,.F.);
#5566=ADVANCED_FACE('',(#849),#538,.T.);
#5567=ADVANCED_FACE('',(#850),#539,.T.);
#5568=ADVANCED_FACE('',(#851),#540,.T.);
#5569=ADVANCED_FACE('',(#852),#541,.T.);
#5570=ADVANCED_FACE('',(#853),#542,.T.);
#5571=ADVANCED_FACE('',(#854),#543,.T.);
#5572=ADVANCED_FACE('',(#855),#544,.F.);
#5573=ADVANCED_FACE('',(#856),#545,.F.);
#5574=ADVANCED_FACE('',(#857),#546,.F.);
#5575=ADVANCED_FACE('',(#858),#547,.F.);
#5576=ADVANCED_FACE('',(#859),#548,.F.);
#5577=ADVANCED_FACE('',(#860),#549,.F.);
#5578=CLOSED_SHELL('',(#5267,#5268,#5269,#5270,#5271,#5272,#5273,#5274,
#5275,#5276,#5277,#5278,#5279,#5280,#5281,#5282,#5283));
#5579=CLOSED_SHELL('',(#5284,#5285,#5286,#5287,#5288,#5289,#5290,#5291,
#5292,#5293,#5294,#5295,#5296,#5297,#5298,#5299,#5300));
#5580=CLOSED_SHELL('',(#5301,#5302,#5303,#5304,#5305,#5306,#5307,#5308));
#5581=CLOSED_SHELL('',(#5309,#5310,#5311,#5312,#5313,#5314,#5315,#5316));
#5582=CLOSED_SHELL('',(#5317,#5318,#5319,#5320,#5321,#5322,#5323,#5324));
#5583=CLOSED_SHELL('',(#5325,#5326,#5327,#5328,#5329,#5330,#5331,#5332,
#5333,#5334,#5335,#5336,#5337,#5338,#5339,#5340,#5341,#5342,#5343,#5344,
#5345,#5346,#5347,#5348,#5349,#5350,#5351,#5352,#5353,#5354,#5355,#5356,
#5357,#5358,#5359,#5360,#5361,#5362,#5363,#5364,#5365,#5366,#5367,#5368,
#5369,#5370,#5371,#5372,#5373,#5374,#5375,#5376,#5377,#5378,#5379,#5380,
#5381,#5382,#5383,#5384,#5385,#5386,#5387,#5388,#5389,#5390,#5391,#5392,
#5393,#5394));
#5584=CLOSED_SHELL('',(#5395,#5396,#5397,#5398,#5399,#5400,#5401,#5402,
#5403,#5404,#5405,#5406,#5407,#5408,#5409,#5410,#5411,#5412,#5413,#5414,
#5415,#5416,#5417,#5418,#5419,#5420,#5421,#5422,#5423,#5424,#5425,#5426,
#5427,#5428,#5429,#5430,#5431,#5432,#5433,#5434,#5435,#5436,#5437,#5438,
#5439,#5440,#5441,#5442,#5443,#5444,#5445,#5446,#5447,#5448,#5449,#5450,
#5451,#5452,#5453,#5454,#5455,#5456,#5457,#5458,#5459,#5460,#5461,#5462,
#5463,#5464,#5465,#5466,#5467,#5468,#5469,#5470,#5471,#5472,#5473,#5474,
#5475,#5476,#5477,#5478,#5479,#5480,#5481,#5482,#5483,#5484,#5485));
#5585=CLOSED_SHELL('',(#5486,#5487,#5488,#5489,#5490,#5491,#5492,#5493));
#5586=CLOSED_SHELL('',(#5494,#5495,#5496,#5497,#5498,#5499,#5500,#5501,
#5502,#5503,#5504,#5505,#5506,#5507,#5508,#5509,#5510,#5511,#5512,#5513,
#5514));
#5587=CLOSED_SHELL('',(#5515,#5516,#5517,#5518,#5519,#5520,#5521,#5522,
#5523,#5524,#5525,#5526,#5527,#5528,#5529,#5530,#5531,#5532,#5533,#5534,
#5535));
#5588=CLOSED_SHELL('',(#5536,#5537,#5538,#5539,#5540,#5541,#5542,#5543,
#5544,#5545,#5546,#5547,#5548,#5549,#5550,#5551,#5552,#5553,#5554,#5555,
#5556));
#5589=CLOSED_SHELL('',(#5557,#5558,#5559,#5560,#5561,#5562,#5563,#5564,
#5565,#5566,#5567,#5568,#5569,#5570,#5571,#5572,#5573,#5574,#5575,#5576,
#5577));
#5590=DERIVED_UNIT_ELEMENT(#5606,1.);
#5591=DERIVED_UNIT_ELEMENT(#12968,-3.);
#5592=DERIVED_UNIT_ELEMENT(#5606,1.);
#5593=DERIVED_UNIT_ELEMENT(#12968,-3.);
#5594=DERIVED_UNIT_ELEMENT(#5606,1.);
#5595=DERIVED_UNIT_ELEMENT(#12968,-3.);
#5596=DERIVED_UNIT_ELEMENT(#5606,1.);
#5597=DERIVED_UNIT_ELEMENT(#12968,-3.);
#5598=DERIVED_UNIT_ELEMENT(#5606,1.);
#5599=DERIVED_UNIT_ELEMENT(#12968,-3.);
#5600=DERIVED_UNIT_ELEMENT(#5606,1.);
#5601=DERIVED_UNIT_ELEMENT(#12968,-3.);
#5602=DERIVED_UNIT_ELEMENT(#5606,1.);
#5603=DERIVED_UNIT_ELEMENT(#12968,-3.);
#5604=DERIVED_UNIT_ELEMENT(#5606,1.);
#5605=DERIVED_UNIT_ELEMENT(#12968,-3.);
#5606=(
MASS_UNIT()
NAMED_UNIT(*)
SI_UNIT(.KILO.,.GRAM.)
);
#5607=DERIVED_UNIT((#5590,#5591));
#5608=DERIVED_UNIT((#5592,#5593));
#5609=DERIVED_UNIT((#5594,#5595));
#5610=DERIVED_UNIT((#5596,#5597));
#5611=DERIVED_UNIT((#5598,#5599));
#5612=DERIVED_UNIT((#5600,#5601));
#5613=DERIVED_UNIT((#5602,#5603));
#5614=DERIVED_UNIT((#5604,#5605));
#5615=MEASURE_REPRESENTATION_ITEM('density measure',
POSITIVE_RATIO_MEASURE(7850.),#5607);
#5616=MEASURE_REPRESENTATION_ITEM('density measure',
POSITIVE_RATIO_MEASURE(7850.),#5608);
#5617=MEASURE_REPRESENTATION_ITEM('density measure',
POSITIVE_RATIO_MEASURE(7850.),#5609);
#5618=MEASURE_REPRESENTATION_ITEM('density measure',
POSITIVE_RATIO_MEASURE(7850.),#5610);
#5619=MEASURE_REPRESENTATION_ITEM('density measure',
POSITIVE_RATIO_MEASURE(7850.),#5611);
#5620=MEASURE_REPRESENTATION_ITEM('density measure',
POSITIVE_RATIO_MEASURE(7850.),#5612);
#5621=MEASURE_REPRESENTATION_ITEM('density measure',
POSITIVE_RATIO_MEASURE(7850.),#5613);
#5622=MEASURE_REPRESENTATION_ITEM('density measure',
POSITIVE_RATIO_MEASURE(7850.),#5614);
#5623=PROPERTY_DEFINITION_REPRESENTATION(#5663,#5639);
#5624=PROPERTY_DEFINITION_REPRESENTATION(#5664,#5640);
#5625=PROPERTY_DEFINITION_REPRESENTATION(#5665,#5641);
#5626=PROPERTY_DEFINITION_REPRESENTATION(#5666,#5642);
#5627=PROPERTY_DEFINITION_REPRESENTATION(#5667,#5643);
#5628=PROPERTY_DEFINITION_REPRESENTATION(#5668,#5644);
#5629=PROPERTY_DEFINITION_REPRESENTATION(#5669,#5645);
#5630=PROPERTY_DEFINITION_REPRESENTATION(#5670,#5646);
#5631=PROPERTY_DEFINITION_REPRESENTATION(#5671,#5647);
#5632=PROPERTY_DEFINITION_REPRESENTATION(#5672,#5648);
#5633=PROPERTY_DEFINITION_REPRESENTATION(#5673,#5649);
#5634=PROPERTY_DEFINITION_REPRESENTATION(#5674,#5650);
#5635=PROPERTY_DEFINITION_REPRESENTATION(#5675,#5651);
#5636=PROPERTY_DEFINITION_REPRESENTATION(#5676,#5652);
#5637=PROPERTY_DEFINITION_REPRESENTATION(#5677,#5653);
#5638=PROPERTY_DEFINITION_REPRESENTATION(#5678,#5654);
#5639=REPRESENTATION('material name',(#5655),#12958);
#5640=REPRESENTATION('density',(#5615),#12958);
#5641=REPRESENTATION('material name',(#5656),#12959);
#5642=REPRESENTATION('density',(#5616),#12959);
#5643=REPRESENTATION('material name',(#5657),#12960);
#5644=REPRESENTATION('density',(#5617),#12960);
#5645=REPRESENTATION('material name',(#5658),#12961);
#5646=REPRESENTATION('density',(#5618),#12961);
#5647=REPRESENTATION('material name',(#5659),#12962);
#5648=REPRESENTATION('density',(#5619),#12962);
#5649=REPRESENTATION('material name',(#5660),#12963);
#5650=REPRESENTATION('density',(#5620),#12963);
#5651=REPRESENTATION('material name',(#5661),#12964);
#5652=REPRESENTATION('density',(#5621),#12964);
#5653=REPRESENTATION('material name',(#5662),#12965);
#5654=REPRESENTATION('density',(#5622),#12965);
#5655=DESCRIPTIVE_REPRESENTATION_ITEM('Steel','Steel');
#5656=DESCRIPTIVE_REPRESENTATION_ITEM('Steel','Steel');
#5657=DESCRIPTIVE_REPRESENTATION_ITEM('Steel','Steel');
#5658=DESCRIPTIVE_REPRESENTATION_ITEM('Steel','Steel');
#5659=DESCRIPTIVE_REPRESENTATION_ITEM('Steel','Steel');
#5660=DESCRIPTIVE_REPRESENTATION_ITEM('Steel','Steel');
#5661=DESCRIPTIVE_REPRESENTATION_ITEM('Steel','Steel');
#5662=DESCRIPTIVE_REPRESENTATION_ITEM('Steel','Steel');
#5663=PROPERTY_DEFINITION('material property','material name',#13035);
#5664=PROPERTY_DEFINITION('material property','density of part',#13035);
#5665=PROPERTY_DEFINITION('material property','material name',#13036);
#5666=PROPERTY_DEFINITION('material property','density of part',#13036);
#5667=PROPERTY_DEFINITION('material property','material name',#13037);
#5668=PROPERTY_DEFINITION('material property','density of part',#13037);
#5669=PROPERTY_DEFINITION('material property','material name',#13038);
#5670=PROPERTY_DEFINITION('material property','density of part',#13038);
#5671=PROPERTY_DEFINITION('material property','material name',#13039);
#5672=PROPERTY_DEFINITION('material property','density of part',#13039);
#5673=PROPERTY_DEFINITION('material property','material name',#13040);
#5674=PROPERTY_DEFINITION('material property','density of part',#13040);
#5675=PROPERTY_DEFINITION('material property','material name',#13041);
#5676=PROPERTY_DEFINITION('material property','density of part',#13041);
#5677=PROPERTY_DEFINITION('material property','material name',#13042);
#5678=PROPERTY_DEFINITION('material property','density of part',#13042);
#5679=AXIS2_PLACEMENT_3D('',#7765,#6222,#6223);
#5680=AXIS2_PLACEMENT_3D('',#7766,#6224,#6225);
#5681=AXIS2_PLACEMENT_3D('',#7767,#6226,#6227);
#5682=AXIS2_PLACEMENT_3D('',#7769,#6228,#6229);
#5683=AXIS2_PLACEMENT_3D('',#7772,#6231,#6232);
#5684=AXIS2_PLACEMENT_3D('',#7773,#6233,#6234);
#5685=AXIS2_PLACEMENT_3D('',#7775,#6235,#6236);
#5686=AXIS2_PLACEMENT_3D('',#7778,#6238,#6239);
#5687=AXIS2_PLACEMENT_3D('',#7779,#6240,#6241);
#5688=AXIS2_PLACEMENT_3D('',#7781,#6242,#6243);
#5689=AXIS2_PLACEMENT_3D('',#7784,#6245,#6246);
#5690=AXIS2_PLACEMENT_3D('',#7785,#6247,#6248);
#5691=AXIS2_PLACEMENT_3D('',#7787,#6249,#6250);
#5692=AXIS2_PLACEMENT_3D('',#7790,#6252,#6253);
#5693=AXIS2_PLACEMENT_3D('',#7791,#6254,#6255);
#5694=AXIS2_PLACEMENT_3D('',#7793,#6256,#6257);
#5695=AXIS2_PLACEMENT_3D('',#7796,#6259,#6260);
#5696=AXIS2_PLACEMENT_3D('',#7797,#6261,#6262);
#5697=AXIS2_PLACEMENT_3D('',#7799,#6263,#6264);
#5698=AXIS2_PLACEMENT_3D('',#7802,#6266,#6267);
#5699=AXIS2_PLACEMENT_3D('',#7803,#6268,#6269);
#5700=AXIS2_PLACEMENT_3D('',#7805,#6270,#6271);
#5701=AXIS2_PLACEMENT_3D('',#7808,#6273,#6274);
#5702=AXIS2_PLACEMENT_3D('',#7809,#6275,#6276);
#5703=AXIS2_PLACEMENT_3D('',#7812,#6277,#6278);
#5704=AXIS2_PLACEMENT_3D('',#7816,#6280,#6281);
#5705=AXIS2_PLACEMENT_3D('',#7818,#6283,#6284);
#5706=AXIS2_PLACEMENT_3D('',#7824,#6288,#6289);
#5707=AXIS2_PLACEMENT_3D('',#7826,#6290,#6291);
#5708=AXIS2_PLACEMENT_3D('',#7829,#6293,#6294);
#5709=AXIS2_PLACEMENT_3D('',#7830,#6295,#6296);
#5710=AXIS2_PLACEMENT_3D('',#7836,#6300,#6301);
#5711=AXIS2_PLACEMENT_3D('',#7838,#6302,#6303);
#5712=AXIS2_PLACEMENT_3D('',#7841,#6305,#6306);
#5713=AXIS2_PLACEMENT_3D('',#7842,#6307,#6308);
#5714=AXIS2_PLACEMENT_3D('',#7848,#6312,#6313);
#5715=AXIS2_PLACEMENT_3D('',#7850,#6314,#6315);
#5716=AXIS2_PLACEMENT_3D('',#7853,#6317,#6318);
#5717=AXIS2_PLACEMENT_3D('',#7854,#6319,#6320);
#5718=AXIS2_PLACEMENT_3D('',#7857,#6323,#6324);
#5719=AXIS2_PLACEMENT_3D('',#7858,#6325,#6326);
#5720=AXIS2_PLACEMENT_3D('',#7859,#6327,#6328);
#5721=AXIS2_PLACEMENT_3D('',#7861,#6329,#6330);
#5722=AXIS2_PLACEMENT_3D('',#7864,#6332,#6333);
#5723=AXIS2_PLACEMENT_3D('',#7865,#6334,#6335);
#5724=AXIS2_PLACEMENT_3D('',#7867,#6336,#6337);
#5725=AXIS2_PLACEMENT_3D('',#7870,#6339,#6340);
#5726=AXIS2_PLACEMENT_3D('',#7871,#6341,#6342);
#5727=AXIS2_PLACEMENT_3D('',#7873,#6343,#6344);
#5728=AXIS2_PLACEMENT_3D('',#7876,#6346,#6347);
#5729=AXIS2_PLACEMENT_3D('',#7877,#6348,#6349);
#5730=AXIS2_PLACEMENT_3D('',#7879,#6350,#6351);
#5731=AXIS2_PLACEMENT_3D('',#7882,#6353,#6354);
#5732=AXIS2_PLACEMENT_3D('',#7883,#6355,#6356);
#5733=AXIS2_PLACEMENT_3D('',#7886,#6357,#6358);
#5734=AXIS2_PLACEMENT_3D('',#7890,#6360,#6361);
#5735=AXIS2_PLACEMENT_3D('',#7892,#6363,#6364);
#5736=AXIS2_PLACEMENT_3D('',#7894,#6365,#6366);
#5737=AXIS2_PLACEMENT_3D('',#7897,#6368,#6369);
#5738=AXIS2_PLACEMENT_3D('',#7898,#6370,#6371);
#5739=AXIS2_PLACEMENT_3D('',#7900,#6372,#6373);
#5740=AXIS2_PLACEMENT_3D('',#7903,#6375,#6376);
#5741=AXIS2_PLACEMENT_3D('',#7904,#6377,#6378);
#5742=AXIS2_PLACEMENT_3D('',#7906,#6379,#6380);
#5743=AXIS2_PLACEMENT_3D('',#7909,#6382,#6383);
#5744=AXIS2_PLACEMENT_3D('',#7910,#6384,#6385);
#5745=AXIS2_PLACEMENT_3D('',#7916,#6389,#6390);
#5746=AXIS2_PLACEMENT_3D('',#7918,#6391,#6392);
#5747=AXIS2_PLACEMENT_3D('',#7921,#6394,#6395);
#5748=AXIS2_PLACEMENT_3D('',#7922,#6396,#6397);
#5749=AXIS2_PLACEMENT_3D('',#7928,#6401,#6402);
#5750=AXIS2_PLACEMENT_3D('',#7930,#6403,#6404);
#5751=AXIS2_PLACEMENT_3D('',#7933,#6406,#6407);
#5752=AXIS2_PLACEMENT_3D('',#7934,#6408,#6409);
#5753=AXIS2_PLACEMENT_3D('',#7940,#6413,#6414);
#5754=AXIS2_PLACEMENT_3D('',#7942,#6415,#6416);
#5755=AXIS2_PLACEMENT_3D('',#7945,#6418,#6419);
#5756=AXIS2_PLACEMENT_3D('',#7946,#6420,#6421);
#5757=AXIS2_PLACEMENT_3D('',#7949,#6424,#6425);
#5758=AXIS2_PLACEMENT_3D('',#7950,#6426,#6427);
#5759=AXIS2_PLACEMENT_3D('',#7951,#6428,#6429);
#5760=AXIS2_PLACEMENT_3D('',#7960,#6434,#6435);
#5761=AXIS2_PLACEMENT_3D('',#7966,#6439,#6440);
#5762=AXIS2_PLACEMENT_3D('',#7972,#6444,#6445);
#5763=AXIS2_PLACEMENT_3D('',#7978,#6449,#6450);
#5764=AXIS2_PLACEMENT_3D('',#7984,#6454,#6455);
#5765=AXIS2_PLACEMENT_3D('',#7987,#6458,#6459);
#5766=AXIS2_PLACEMENT_3D('',#7988,#6460,#6461);
#5767=AXIS2_PLACEMENT_3D('',#7989,#6462,#6463);
#5768=AXIS2_PLACEMENT_3D('',#7998,#6468,#6469);
#5769=AXIS2_PLACEMENT_3D('',#8004,#6473,#6474);
#5770=AXIS2_PLACEMENT_3D('',#8010,#6478,#6479);
#5771=AXIS2_PLACEMENT_3D('',#8016,#6483,#6484);
#5772=AXIS2_PLACEMENT_3D('',#8022,#6488,#6489);
#5773=AXIS2_PLACEMENT_3D('',#8025,#6492,#6493);
#5774=AXIS2_PLACEMENT_3D('',#8026,#6494,#6495);
#5775=AXIS2_PLACEMENT_3D('',#8027,#6496,#6497);
#5776=AXIS2_PLACEMENT_3D('',#8036,#6502,#6503);
#5777=AXIS2_PLACEMENT_3D('',#8042,#6507,#6508);
#5778=AXIS2_PLACEMENT_3D('',#8048,#6512,#6513);
#5779=AXIS2_PLACEMENT_3D('',#8054,#6517,#6518);
#5780=AXIS2_PLACEMENT_3D('',#8060,#6522,#6523);
#5781=AXIS2_PLACEMENT_3D('',#8063,#6526,#6527);
#5782=AXIS2_PLACEMENT_3D('',#8064,#6528,#6529);
#5783=AXIS2_PLACEMENT_3D('',#8065,#6530,#6531);
#5784=AXIS2_PLACEMENT_3D('',#8066,#6532,#6533);
#5785=AXIS2_PLACEMENT_3D('',#8068,#6534,#6535);
#5786=AXIS2_PLACEMENT_3D('',#8071,#6537,#6538);
#5787=AXIS2_PLACEMENT_3D('',#8072,#6539,#6540);
#5788=AXIS2_PLACEMENT_3D('',#8075,#6541,#6542);
#5789=AXIS2_PLACEMENT_3D('',#8079,#6544,#6545);
#5790=AXIS2_PLACEMENT_3D('',#8081,#6547,#6548);
#5791=AXIS2_PLACEMENT_3D('',#8083,#6549,#6550);
#5792=AXIS2_PLACEMENT_3D('',#8086,#6552,#6553);
#5793=AXIS2_PLACEMENT_3D('',#8087,#6554,#6555);
#5794=AXIS2_PLACEMENT_3D('',#8089,#6556,#6557);
#5795=AXIS2_PLACEMENT_3D('',#8092,#6559,#6560);
#5796=AXIS2_PLACEMENT_3D('',#8093,#6561,#6562);
#5797=AXIS2_PLACEMENT_3D('',#8095,#6563,#6564);
#5798=AXIS2_PLACEMENT_3D('',#8098,#6566,#6567);
#5799=AXIS2_PLACEMENT_3D('',#8099,#6568,#6569);
#5800=AXIS2_PLACEMENT_3D('',#8100,#6570,#6571);
#5801=AXIS2_PLACEMENT_3D('',#8101,#6572,#6573);
#5802=AXIS2_PLACEMENT_3D('',#8108,#6576,#6577);
#5803=AXIS2_PLACEMENT_3D('',#8112,#6579,#6580);
#5804=AXIS2_PLACEMENT_3D('',#8126,#6587,#6588);
#5805=AXIS2_PLACEMENT_3D('',#8144,#6597,#6598);
#5806=AXIS2_PLACEMENT_3D('',#8154,#6603,#6604);
#5807=AXIS2_PLACEMENT_3D('',#8166,#6610,#6611);
#5808=AXIS2_PLACEMENT_3D('',#8177,#6617,#6618);
#5809=AXIS2_PLACEMENT_3D('',#8178,#6619,#6620);
#5810=AXIS2_PLACEMENT_3D('',#8199,#6630,#6631);
#5811=AXIS2_PLACEMENT_3D('',#8213,#6638,#6639);
#5812=AXIS2_PLACEMENT_3D('',#8217,#6641,#6642);
#5813=AXIS2_PLACEMENT_3D('',#8228,#6648,#6649);
#5814=AXIS2_PLACEMENT_3D('',#8237,#6653,#6654);
#5815=AXIS2_PLACEMENT_3D('',#8244,#6658,#6659);
#5816=AXIS2_PLACEMENT_3D('',#8252,#6664,#6665);
#5817=AXIS2_PLACEMENT_3D('',#8255,#6668,#6669);
#5818=AXIS2_PLACEMENT_3D('',#8257,#6671,#6672);
#5819=AXIS2_PLACEMENT_3D('',#8259,#6674,#6675);
#5820=AXIS2_PLACEMENT_3D('',#8261,#6677,#6678);
#5821=AXIS2_PLACEMENT_3D('',#8263,#6680,#6681);
#5822=AXIS2_PLACEMENT_3D('',#8265,#6683,#6684);
#5823=AXIS2_PLACEMENT_3D('',#8267,#6686,#6687);
#5824=AXIS2_PLACEMENT_3D('',#8269,#6689,#6690);
#5825=AXIS2_PLACEMENT_3D('',#8271,#6692,#6693);
#5826=AXIS2_PLACEMENT_3D('',#8273,#6695,#6696);
#5827=AXIS2_PLACEMENT_3D('',#8275,#6698,#6699);
#5828=AXIS2_PLACEMENT_3D('',#8277,#6701,#6702);
#5829=AXIS2_PLACEMENT_3D('',#8279,#6704,#6705);
#5830=AXIS2_PLACEMENT_3D('',#8281,#6707,#6708);
#5831=AXIS2_PLACEMENT_3D('',#8283,#6710,#6711);
#5832=AXIS2_PLACEMENT_3D('',#8285,#6713,#6714);
#5833=AXIS2_PLACEMENT_3D('',#8287,#6716,#6717);
#5834=AXIS2_PLACEMENT_3D('',#8289,#6719,#6720);
#5835=AXIS2_PLACEMENT_3D('',#8291,#6722,#6723);
#5836=AXIS2_PLACEMENT_3D('',#8292,#6724,#6725);
#5837=AXIS2_PLACEMENT_3D('',#8298,#6729,#6730);
#5838=AXIS2_PLACEMENT_3D('',#8302,#6733,#6734);
#5839=AXIS2_PLACEMENT_3D('',#8306,#6737,#6738);
#5840=AXIS2_PLACEMENT_3D('',#8310,#6741,#6742);
#5841=AXIS2_PLACEMENT_3D('',#8311,#6743,#6744);
#5842=AXIS2_PLACEMENT_3D('',#8312,#6745,#6746);
#5843=AXIS2_PLACEMENT_3D('',#8313,#6747,#6748);
#5844=AXIS2_PLACEMENT_3D('',#8319,#6752,#6753);
#5845=AXIS2_PLACEMENT_3D('',#8323,#6756,#6757);
#5846=AXIS2_PLACEMENT_3D('',#8327,#6760,#6761);
#5847=AXIS2_PLACEMENT_3D('',#8329,#6762,#6763);
#5848=AXIS2_PLACEMENT_3D('',#8331,#6765,#6766);
#5849=AXIS2_PLACEMENT_3D('',#8333,#6768,#6769);
#5850=AXIS2_PLACEMENT_3D('',#8334,#6770,#6771);
#5851=AXIS2_PLACEMENT_3D('',#8338,#6773,#6774);
#5852=AXIS2_PLACEMENT_3D('',#8340,#6776,#6777);
#5853=AXIS2_PLACEMENT_3D('',#8344,#6780,#6781);
#5854=AXIS2_PLACEMENT_3D('',#8348,#6784,#6785);
#5855=AXIS2_PLACEMENT_3D('',#8352,#6788,#6789);
#5856=AXIS2_PLACEMENT_3D('',#8356,#6792,#6793);
#5857=AXIS2_PLACEMENT_3D('',#8358,#6794,#6795);
#5858=AXIS2_PLACEMENT_3D('',#8360,#6797,#6798);
#5859=AXIS2_PLACEMENT_3D('',#8364,#6801,#6802);
#5860=AXIS2_PLACEMENT_3D('',#8366,#6804,#6805);
#5861=AXIS2_PLACEMENT_3D('',#8367,#6806,#6807);
#5862=AXIS2_PLACEMENT_3D('',#8371,#6810,#6811);
#5863=AXIS2_PLACEMENT_3D('',#8375,#6814,#6815);
#5864=AXIS2_PLACEMENT_3D('',#8377,#6816,#6817);
#5865=AXIS2_PLACEMENT_3D('',#8379,#6819,#6820);
#5866=AXIS2_PLACEMENT_3D('',#8383,#6823,#6824);
#5867=AXIS2_PLACEMENT_3D('',#8387,#6827,#6828);
#5868=AXIS2_PLACEMENT_3D('',#8391,#6831,#6832);
#5869=AXIS2_PLACEMENT_3D('',#8393,#6834,#6835);
#5870=AXIS2_PLACEMENT_3D('',#8394,#6836,#6837);
#5871=AXIS2_PLACEMENT_3D('',#8400,#6841,#6842);
#5872=AXIS2_PLACEMENT_3D('',#8404,#6845,#6846);
#5873=AXIS2_PLACEMENT_3D('',#8406,#6847,#6848);
#5874=AXIS2_PLACEMENT_3D('',#8408,#6850,#6851);
#5875=AXIS2_PLACEMENT_3D('',#8412,#6854,#6855);
#5876=AXIS2_PLACEMENT_3D('',#8414,#6857,#6858);
#5877=AXIS2_PLACEMENT_3D('',#8415,#6859,#6860);
#5878=AXIS2_PLACEMENT_3D('',#8421,#6864,#6865);
#5879=AXIS2_PLACEMENT_3D('',#8425,#6868,#6869);
#5880=AXIS2_PLACEMENT_3D('',#8429,#6872,#6873);
#5881=AXIS2_PLACEMENT_3D('',#8431,#6874,#6875);
#5882=AXIS2_PLACEMENT_3D('',#8433,#6877,#6878);
#5883=AXIS2_PLACEMENT_3D('',#8435,#6880,#6881);
#5884=AXIS2_PLACEMENT_3D('',#8436,#6882,#6883);
#5885=AXIS2_PLACEMENT_3D('',#8437,#6884,#6885);
#5886=AXIS2_PLACEMENT_3D('',#8439,#6886,#6887);
#5887=AXIS2_PLACEMENT_3D('',#8442,#6889,#6890);
#5888=AXIS2_PLACEMENT_3D('',#8443,#6891,#6892);
#5889=AXIS2_PLACEMENT_3D('',#8445,#6893,#6894);
#5890=AXIS2_PLACEMENT_3D('',#8448,#6896,#6897);
#5891=AXIS2_PLACEMENT_3D('',#8449,#6898,#6899);
#5892=AXIS2_PLACEMENT_3D('',#8451,#6900,#6901);
#5893=AXIS2_PLACEMENT_3D('',#8454,#6903,#6904);
#5894=AXIS2_PLACEMENT_3D('',#8455,#6905,#6906);
#5895=AXIS2_PLACEMENT_3D('',#8457,#6907,#6908);
#5896=AXIS2_PLACEMENT_3D('',#8460,#6910,#6911);
#5897=AXIS2_PLACEMENT_3D('',#8461,#6912,#6913);
#5898=AXIS2_PLACEMENT_3D('',#8463,#6914,#6915);
#5899=AXIS2_PLACEMENT_3D('',#8466,#6917,#6918);
#5900=AXIS2_PLACEMENT_3D('',#8467,#6919,#6920);
#5901=AXIS2_PLACEMENT_3D('',#8470,#6921,#6922);
#5902=AXIS2_PLACEMENT_3D('',#8474,#6924,#6925);
#5903=AXIS2_PLACEMENT_3D('',#8476,#6927,#6928);
#5904=AXIS2_PLACEMENT_3D('',#8477,#6929,#6930);
#5905=AXIS2_PLACEMENT_3D('',#8478,#6931,#6932);
#5906=AXIS2_PLACEMENT_3D('',#8505,#6933,#6934);
#5907=AXIS2_PLACEMENT_3D('',#8531,#6935,#6936);
#5908=AXIS2_PLACEMENT_3D('',#8557,#6937,#6938);
#5909=AXIS2_PLACEMENT_3D('',#8583,#6939,#6940);
#5910=AXIS2_PLACEMENT_3D('',#8609,#6941,#6942);
#5911=AXIS2_PLACEMENT_3D('',#8635,#6943,#6944);
#5912=AXIS2_PLACEMENT_3D('',#8661,#6945,#6946);
#5913=AXIS2_PLACEMENT_3D('',#8687,#6947,#6948);
#5914=AXIS2_PLACEMENT_3D('',#8713,#6949,#6950);
#5915=AXIS2_PLACEMENT_3D('',#8739,#6951,#6952);
#5916=AXIS2_PLACEMENT_3D('',#8765,#6953,#6954);
#5917=AXIS2_PLACEMENT_3D('',#8791,#6955,#6956);
#5918=AXIS2_PLACEMENT_3D('',#8817,#6957,#6958);
#5919=AXIS2_PLACEMENT_3D('',#8843,#6959,#6960);
#5920=AXIS2_PLACEMENT_3D('',#8869,#6961,#6962);
#5921=AXIS2_PLACEMENT_3D('',#8895,#6963,#6964);
#5922=AXIS2_PLACEMENT_3D('',#8921,#6965,#6966);
#5923=AXIS2_PLACEMENT_3D('',#8970,#6967,#6968);
#5924=AXIS2_PLACEMENT_3D('',#8996,#6969,#6970);
#5925=AXIS2_PLACEMENT_3D('',#9022,#6971,#6972);
#5926=AXIS2_PLACEMENT_3D('',#9048,#6973,#6974);
#5927=AXIS2_PLACEMENT_3D('',#9074,#6975,#6976);
#5928=AXIS2_PLACEMENT_3D('',#9100,#6977,#6978);
#5929=AXIS2_PLACEMENT_3D('',#9126,#6979,#6980);
#5930=AXIS2_PLACEMENT_3D('',#9152,#6981,#6982);
#5931=AXIS2_PLACEMENT_3D('',#9178,#6983,#6984);
#5932=AXIS2_PLACEMENT_3D('',#9204,#6985,#6986);
#5933=AXIS2_PLACEMENT_3D('',#9230,#6987,#6988);
#5934=AXIS2_PLACEMENT_3D('',#9256,#6989,#6990);
#5935=AXIS2_PLACEMENT_3D('',#9282,#6991,#6992);
#5936=AXIS2_PLACEMENT_3D('',#9308,#6993,#6994);
#5937=AXIS2_PLACEMENT_3D('',#9334,#6995,#6996);
#5938=AXIS2_PLACEMENT_3D('',#9360,#6997,#6998);
#5939=AXIS2_PLACEMENT_3D('',#9386,#6999,#7000);
#5940=AXIS2_PLACEMENT_3D('',#9412,#7001,#7002);
#5941=AXIS2_PLACEMENT_3D('',#9438,#7003,#7004);
#5942=AXIS2_PLACEMENT_3D('',#9464,#7005,#7006);
#5943=AXIS2_PLACEMENT_3D('',#9490,#7007,#7008);
#5944=AXIS2_PLACEMENT_3D('',#9515,#7009,#7010);
#5945=AXIS2_PLACEMENT_3D('',#9516,#7011,#7012);
#5946=AXIS2_PLACEMENT_3D('',#9543,#7013,#7014);
#5947=AXIS2_PLACEMENT_3D('',#9569,#7015,#7016);
#5948=AXIS2_PLACEMENT_3D('',#9595,#7017,#7018);
#5949=AXIS2_PLACEMENT_3D('',#9621,#7019,#7020);
#5950=AXIS2_PLACEMENT_3D('',#9647,#7021,#7022);
#5951=AXIS2_PLACEMENT_3D('',#9673,#7023,#7024);
#5952=AXIS2_PLACEMENT_3D('',#9699,#7025,#7026);
#5953=AXIS2_PLACEMENT_3D('',#9725,#7027,#7028);
#5954=AXIS2_PLACEMENT_3D('',#9751,#7029,#7030);
#5955=AXIS2_PLACEMENT_3D('',#9777,#7031,#7032);
#5956=AXIS2_PLACEMENT_3D('',#9803,#7033,#7034);
#5957=AXIS2_PLACEMENT_3D('',#9829,#7035,#7036);
#5958=AXIS2_PLACEMENT_3D('',#9855,#7037,#7038);
#5959=AXIS2_PLACEMENT_3D('',#9881,#7039,#7040);
#5960=AXIS2_PLACEMENT_3D('',#9907,#7041,#7042);
#5961=AXIS2_PLACEMENT_3D('',#9933,#7043,#7044);
#5962=AXIS2_PLACEMENT_3D('',#9959,#7045,#7046);
#5963=AXIS2_PLACEMENT_3D('',#9985,#7047,#7048);
#5964=AXIS2_PLACEMENT_3D('',#10011,#7049,#7050);
#5965=AXIS2_PLACEMENT_3D('',#10037,#7051,#7052);
#5966=AXIS2_PLACEMENT_3D('',#10063,#7053,#7054);
#5967=AXIS2_PLACEMENT_3D('',#10089,#7055,#7056);
#5968=AXIS2_PLACEMENT_3D('',#10138,#7057,#7058);
#5969=AXIS2_PLACEMENT_3D('',#10164,#7059,#7060);
#5970=AXIS2_PLACEMENT_3D('',#10190,#7061,#7062);
#5971=AXIS2_PLACEMENT_3D('',#10216,#7063,#7064);
#5972=AXIS2_PLACEMENT_3D('',#10242,#7065,#7066);
#5973=AXIS2_PLACEMENT_3D('',#10268,#7067,#7068);
#5974=AXIS2_PLACEMENT_3D('',#10294,#7069,#7070);
#5975=AXIS2_PLACEMENT_3D('',#10320,#7071,#7072);
#5976=AXIS2_PLACEMENT_3D('',#10346,#7073,#7074);
#5977=AXIS2_PLACEMENT_3D('',#10372,#7075,#7076);
#5978=AXIS2_PLACEMENT_3D('',#10398,#7077,#7078);
#5979=AXIS2_PLACEMENT_3D('',#10424,#7079,#7080);
#5980=AXIS2_PLACEMENT_3D('',#10450,#7081,#7082);
#5981=AXIS2_PLACEMENT_3D('',#10476,#7083,#7084);
#5982=AXIS2_PLACEMENT_3D('',#10502,#7085,#7086);
#5983=AXIS2_PLACEMENT_3D('',#10528,#7087,#7088);
#5984=AXIS2_PLACEMENT_3D('',#10553,#7089,#7090);
#5985=AXIS2_PLACEMENT_3D('',#10602,#7093,#7094);
#5986=AXIS2_PLACEMENT_3D('',#10651,#7097,#7098);
#5987=AXIS2_PLACEMENT_3D('',#10700,#7101,#7102);
#5988=AXIS2_PLACEMENT_3D('',#10749,#7105,#7106);
#5989=AXIS2_PLACEMENT_3D('',#10798,#7109,#7110);
#5990=AXIS2_PLACEMENT_3D('',#10847,#7113,#7114);
#5991=AXIS2_PLACEMENT_3D('',#10896,#7117,#7118);
#5992=AXIS2_PLACEMENT_3D('',#10945,#7121,#7122);
#5993=AXIS2_PLACEMENT_3D('',#10994,#7125,#7126);
#5994=AXIS2_PLACEMENT_3D('',#11043,#7129,#7130);
#5995=AXIS2_PLACEMENT_3D('',#11092,#7133,#7134);
#5996=AXIS2_PLACEMENT_3D('',#11141,#7137,#7138);
#5997=AXIS2_PLACEMENT_3D('',#11190,#7141,#7142);
#5998=AXIS2_PLACEMENT_3D('',#11239,#7145,#7146);
#5999=AXIS2_PLACEMENT_3D('',#11288,#7149,#7150);
#6000=AXIS2_PLACEMENT_3D('',#11337,#7153,#7154);
#6001=AXIS2_PLACEMENT_3D('',#11386,#7157,#7158);
#6002=AXIS2_PLACEMENT_3D('',#11481,#7161,#7162);
#6003=AXIS2_PLACEMENT_3D('',#11530,#7165,#7166);
#6004=AXIS2_PLACEMENT_3D('',#11579,#7169,#7170);
#6005=AXIS2_PLACEMENT_3D('',#11628,#7173,#7174);
#6006=AXIS2_PLACEMENT_3D('',#11677,#7177,#7178);
#6007=AXIS2_PLACEMENT_3D('',#11726,#7181,#7182);
#6008=AXIS2_PLACEMENT_3D('',#11775,#7185,#7186);
#6009=AXIS2_PLACEMENT_3D('',#11824,#7189,#7190);
#6010=AXIS2_PLACEMENT_3D('',#11873,#7193,#7194);
#6011=AXIS2_PLACEMENT_3D('',#11922,#7197,#7198);
#6012=AXIS2_PLACEMENT_3D('',#11971,#7201,#7202);
#6013=AXIS2_PLACEMENT_3D('',#12020,#7205,#7206);
#6014=AXIS2_PLACEMENT_3D('',#12069,#7209,#7210);
#6015=AXIS2_PLACEMENT_3D('',#12118,#7213,#7214);
#6016=AXIS2_PLACEMENT_3D('',#12167,#7217,#7218);
#6017=AXIS2_PLACEMENT_3D('',#12216,#7221,#7222);
#6018=AXIS2_PLACEMENT_3D('',#12265,#7225,#7226);
#6019=AXIS2_PLACEMENT_3D('',#12314,#7229,#7230);
#6020=AXIS2_PLACEMENT_3D('',#12363,#7233,#7234);
#6021=AXIS2_PLACEMENT_3D('',#12412,#7237,#7238);
#6022=AXIS2_PLACEMENT_3D('',#12461,#7241,#7242);
#6023=AXIS2_PLACEMENT_3D('',#12510,#7245,#7246);
#6024=AXIS2_PLACEMENT_3D('',#12511,#7247,#7248);
#6025=AXIS2_PLACEMENT_3D('',#12512,#7249,#7250);
#6026=AXIS2_PLACEMENT_3D('',#12513,#7251,#7252);
#6027=AXIS2_PLACEMENT_3D('',#12514,#7253,#7254);
#6028=AXIS2_PLACEMENT_3D('',#12516,#7255,#7256);
#6029=AXIS2_PLACEMENT_3D('',#12519,#7258,#7259);
#6030=AXIS2_PLACEMENT_3D('',#12520,#7260,#7261);
#6031=AXIS2_PLACEMENT_3D('',#12522,#7262,#7263);
#6032=AXIS2_PLACEMENT_3D('',#12525,#7265,#7266);
#6033=AXIS2_PLACEMENT_3D('',#12526,#7267,#7268);
#6034=AXIS2_PLACEMENT_3D('',#12529,#7269,#7270);
#6035=AXIS2_PLACEMENT_3D('',#12533,#7272,#7273);
#6036=AXIS2_PLACEMENT_3D('',#12535,#7275,#7276);
#6037=AXIS2_PLACEMENT_3D('',#12538,#7277,#7278);
#6038=AXIS2_PLACEMENT_3D('',#12542,#7280,#7281);
#6039=AXIS2_PLACEMENT_3D('',#12544,#7283,#7284);
#6040=AXIS2_PLACEMENT_3D('',#12547,#7287,#7288);
#6041=AXIS2_PLACEMENT_3D('',#12549,#7290,#7291);
#6042=AXIS2_PLACEMENT_3D('',#12551,#7293,#7294);
#6043=AXIS2_PLACEMENT_3D('',#12552,#7295,#7296);
#6044=AXIS2_PLACEMENT_3D('',#12553,#7297,#7298);
#6045=AXIS2_PLACEMENT_3D('',#12558,#7300,#7301);
#6046=AXIS2_PLACEMENT_3D('',#12560,#7302,#7303);
#6047=AXIS2_PLACEMENT_3D('',#12562,#7304,#7305);
#6048=AXIS2_PLACEMENT_3D('',#12564,#7306,#7307);
#6049=AXIS2_PLACEMENT_3D('',#12566,#7308,#7309);
#6050=AXIS2_PLACEMENT_3D('',#12567,#7310,#7311);
#6051=AXIS2_PLACEMENT_3D('',#12568,#7312,#7313);
#6052=AXIS2_PLACEMENT_3D('',#12570,#7314,#7315);
#6053=AXIS2_PLACEMENT_3D('',#12572,#7316,#7317);
#6054=AXIS2_PLACEMENT_3D('',#12573,#7318,#7319);
#6055=AXIS2_PLACEMENT_3D('',#12574,#7320,#7321);
#6056=AXIS2_PLACEMENT_3D('',#12576,#7322,#7323);
#6057=AXIS2_PLACEMENT_3D('',#12579,#7325,#7326);
#6058=AXIS2_PLACEMENT_3D('',#12580,#7327,#7328);
#6059=AXIS2_PLACEMENT_3D('',#12582,#7330,#7331);
#6060=AXIS2_PLACEMENT_3D('',#12584,#7332,#7333);
#6061=AXIS2_PLACEMENT_3D('',#12587,#7335,#7336);
#6062=AXIS2_PLACEMENT_3D('',#12588,#7337,#7338);
#6063=AXIS2_PLACEMENT_3D('',#12590,#7339,#7340);
#6064=AXIS2_PLACEMENT_3D('',#12591,#7341,#7342);
#6065=AXIS2_PLACEMENT_3D('',#12604,#7349,#7350);
#6066=AXIS2_PLACEMENT_3D('',#12605,#7351,#7352);
#6067=AXIS2_PLACEMENT_3D('',#12606,#7353,#7354);
#6068=AXIS2_PLACEMENT_3D('',#12613,#7359,#7360);
#6069=AXIS2_PLACEMENT_3D('',#12618,#7364,#7365);
#6070=AXIS2_PLACEMENT_3D('',#12623,#7369,#7370);
#6071=AXIS2_PLACEMENT_3D('',#12628,#7374,#7375);
#6072=AXIS2_PLACEMENT_3D('',#12633,#7379,#7380);
#6073=AXIS2_PLACEMENT_3D('',#12636,#7383,#7384);
#6074=AXIS2_PLACEMENT_3D('',#12637,#7385,#7386);
#6075=AXIS2_PLACEMENT_3D('',#12638,#7387,#7388);
#6076=AXIS2_PLACEMENT_3D('',#12639,#7389,#7390);
#6077=AXIS2_PLACEMENT_3D('',#12640,#7391,#7392);
#6078=AXIS2_PLACEMENT_3D('',#12641,#7393,#7394);
#6079=AXIS2_PLACEMENT_3D('',#12642,#7395,#7396);
#6080=AXIS2_PLACEMENT_3D('',#12643,#7397,#7398);
#6081=AXIS2_PLACEMENT_3D('',#12648,#7400,#7401);
#6082=AXIS2_PLACEMENT_3D('',#12650,#7402,#7403);
#6083=AXIS2_PLACEMENT_3D('',#12652,#7404,#7405);
#6084=AXIS2_PLACEMENT_3D('',#12654,#7406,#7407);
#6085=AXIS2_PLACEMENT_3D('',#12656,#7408,#7409);
#6086=AXIS2_PLACEMENT_3D('',#12657,#7410,#7411);
#6087=AXIS2_PLACEMENT_3D('',#12658,#7412,#7413);
#6088=AXIS2_PLACEMENT_3D('',#12660,#7414,#7415);
#6089=AXIS2_PLACEMENT_3D('',#12662,#7416,#7417);
#6090=AXIS2_PLACEMENT_3D('',#12663,#7418,#7419);
#6091=AXIS2_PLACEMENT_3D('',#12664,#7420,#7421);
#6092=AXIS2_PLACEMENT_3D('',#12666,#7422,#7423);
#6093=AXIS2_PLACEMENT_3D('',#12669,#7425,#7426);
#6094=AXIS2_PLACEMENT_3D('',#12670,#7427,#7428);
#6095=AXIS2_PLACEMENT_3D('',#12672,#7430,#7431);
#6096=AXIS2_PLACEMENT_3D('',#12674,#7432,#7433);
#6097=AXIS2_PLACEMENT_3D('',#12677,#7435,#7436);
#6098=AXIS2_PLACEMENT_3D('',#12678,#7437,#7438);
#6099=AXIS2_PLACEMENT_3D('',#12680,#7439,#7440);
#6100=AXIS2_PLACEMENT_3D('',#12681,#7441,#7442);
#6101=AXIS2_PLACEMENT_3D('',#12694,#7449,#7450);
#6102=AXIS2_PLACEMENT_3D('',#12695,#7451,#7452);
#6103=AXIS2_PLACEMENT_3D('',#12696,#7453,#7454);
#6104=AXIS2_PLACEMENT_3D('',#12703,#7459,#7460);
#6105=AXIS2_PLACEMENT_3D('',#12708,#7464,#7465);
#6106=AXIS2_PLACEMENT_3D('',#12713,#7469,#7470);
#6107=AXIS2_PLACEMENT_3D('',#12718,#7474,#7475);
#6108=AXIS2_PLACEMENT_3D('',#12723,#7479,#7480);
#6109=AXIS2_PLACEMENT_3D('',#12726,#7483,#7484);
#6110=AXIS2_PLACEMENT_3D('',#12727,#7485,#7486);
#6111=AXIS2_PLACEMENT_3D('',#12728,#7487,#7488);
#6112=AXIS2_PLACEMENT_3D('',#12729,#7489,#7490);
#6113=AXIS2_PLACEMENT_3D('',#12730,#7491,#7492);
#6114=AXIS2_PLACEMENT_3D('',#12731,#7493,#7494);
#6115=AXIS2_PLACEMENT_3D('',#12732,#7495,#7496);
#6116=AXIS2_PLACEMENT_3D('',#12733,#7497,#7498);
#6117=AXIS2_PLACEMENT_3D('',#12738,#7500,#7501);
#6118=AXIS2_PLACEMENT_3D('',#12740,#7502,#7503);
#6119=AXIS2_PLACEMENT_3D('',#12742,#7504,#7505);
#6120=AXIS2_PLACEMENT_3D('',#12744,#7506,#7507);
#6121=AXIS2_PLACEMENT_3D('',#12746,#7508,#7509);
#6122=AXIS2_PLACEMENT_3D('',#12747,#7510,#7511);
#6123=AXIS2_PLACEMENT_3D('',#12748,#7512,#7513);
#6124=AXIS2_PLACEMENT_3D('',#12750,#7514,#7515);
#6125=AXIS2_PLACEMENT_3D('',#12752,#7516,#7517);
#6126=AXIS2_PLACEMENT_3D('',#12753,#7518,#7519);
#6127=AXIS2_PLACEMENT_3D('',#12754,#7520,#7521);
#6128=AXIS2_PLACEMENT_3D('',#12756,#7522,#7523);
#6129=AXIS2_PLACEMENT_3D('',#12759,#7525,#7526);
#6130=AXIS2_PLACEMENT_3D('',#12760,#7527,#7528);
#6131=AXIS2_PLACEMENT_3D('',#12762,#7530,#7531);
#6132=AXIS2_PLACEMENT_3D('',#12764,#7532,#7533);
#6133=AXIS2_PLACEMENT_3D('',#12767,#7535,#7536);
#6134=AXIS2_PLACEMENT_3D('',#12768,#7537,#7538);
#6135=AXIS2_PLACEMENT_3D('',#12770,#7539,#7540);
#6136=AXIS2_PLACEMENT_3D('',#12771,#7541,#7542);
#6137=AXIS2_PLACEMENT_3D('',#12784,#7549,#7550);
#6138=AXIS2_PLACEMENT_3D('',#12785,#7551,#7552);
#6139=AXIS2_PLACEMENT_3D('',#12786,#7553,#7554);
#6140=AXIS2_PLACEMENT_3D('',#12793,#7559,#7560);
#6141=AXIS2_PLACEMENT_3D('',#12798,#7564,#7565);
#6142=AXIS2_PLACEMENT_3D('',#12803,#7569,#7570);
#6143=AXIS2_PLACEMENT_3D('',#12808,#7574,#7575);
#6144=AXIS2_PLACEMENT_3D('',#12813,#7579,#7580);
#6145=AXIS2_PLACEMENT_3D('',#12816,#7583,#7584);
#6146=AXIS2_PLACEMENT_3D('',#12817,#7585,#7586);
#6147=AXIS2_PLACEMENT_3D('',#12818,#7587,#7588);
#6148=AXIS2_PLACEMENT_3D('',#12819,#7589,#7590);
#6149=AXIS2_PLACEMENT_3D('',#12820,#7591,#7592);
#6150=AXIS2_PLACEMENT_3D('',#12821,#7593,#7594);
#6151=AXIS2_PLACEMENT_3D('',#12822,#7595,#7596);
#6152=AXIS2_PLACEMENT_3D('',#12823,#7597,#7598);
#6153=AXIS2_PLACEMENT_3D('',#12828,#7600,#7601);
#6154=AXIS2_PLACEMENT_3D('',#12830,#7602,#7603);
#6155=AXIS2_PLACEMENT_3D('',#12832,#7604,#7605);
#6156=AXIS2_PLACEMENT_3D('',#12834,#7606,#7607);
#6157=AXIS2_PLACEMENT_3D('',#12836,#7608,#7609);
#6158=AXIS2_PLACEMENT_3D('',#12837,#7610,#7611);
#6159=AXIS2_PLACEMENT_3D('',#12838,#7612,#7613);
#6160=AXIS2_PLACEMENT_3D('',#12840,#7614,#7615);
#6161=AXIS2_PLACEMENT_3D('',#12842,#7616,#7617);
#6162=AXIS2_PLACEMENT_3D('',#12843,#7618,#7619);
#6163=AXIS2_PLACEMENT_3D('',#12844,#7620,#7621);
#6164=AXIS2_PLACEMENT_3D('',#12846,#7622,#7623);
#6165=AXIS2_PLACEMENT_3D('',#12849,#7625,#7626);
#6166=AXIS2_PLACEMENT_3D('',#12850,#7627,#7628);
#6167=AXIS2_PLACEMENT_3D('',#12852,#7630,#7631);
#6168=AXIS2_PLACEMENT_3D('',#12854,#7632,#7633);
#6169=AXIS2_PLACEMENT_3D('',#12857,#7635,#7636);
#6170=AXIS2_PLACEMENT_3D('',#12858,#7637,#7638);
#6171=AXIS2_PLACEMENT_3D('',#12860,#7639,#7640);
#6172=AXIS2_PLACEMENT_3D('',#12861,#7641,#7642);
#6173=AXIS2_PLACEMENT_3D('',#12874,#7649,#7650);
#6174=AXIS2_PLACEMENT_3D('',#12875,#7651,#7652);
#6175=AXIS2_PLACEMENT_3D('',#12876,#7653,#7654);
#6176=AXIS2_PLACEMENT_3D('',#12883,#7659,#7660);
#6177=AXIS2_PLACEMENT_3D('',#12888,#7664,#7665);
#6178=AXIS2_PLACEMENT_3D('',#12893,#7669,#7670);
#6179=AXIS2_PLACEMENT_3D('',#12898,#7674,#7675);
#6180=AXIS2_PLACEMENT_3D('',#12903,#7679,#7680);
#6181=AXIS2_PLACEMENT_3D('',#12906,#7683,#7684);
#6182=AXIS2_PLACEMENT_3D('',#12907,#7685,#7686);
#6183=AXIS2_PLACEMENT_3D('',#12908,#7687,#7688);
#6184=AXIS2_PLACEMENT_3D('',#12909,#7689,#7690);
#6185=AXIS2_PLACEMENT_3D('',#12910,#7691,#7692);
#6186=AXIS2_PLACEMENT_3D('',#12911,#7693,#7694);
#6187=AXIS2_PLACEMENT_3D('',#12912,#7695,#7696);
#6188=AXIS2_PLACEMENT_3D('',#12913,#7697,#7698);
#6189=AXIS2_PLACEMENT_3D('',#12914,#7699,#7700);
#6190=AXIS2_PLACEMENT_3D('',#12915,#7701,#7702);
#6191=AXIS2_PLACEMENT_3D('',#12916,#7703,#7704);
#6192=AXIS2_PLACEMENT_3D('',#12917,#7705,#7706);
#6193=AXIS2_PLACEMENT_3D('',#12918,#7707,#7708);
#6194=AXIS2_PLACEMENT_3D('',#12919,#7709,#7710);
#6195=AXIS2_PLACEMENT_3D('',#12920,#7711,#7712);
#6196=AXIS2_PLACEMENT_3D('',#12921,#7713,#7714);
#6197=AXIS2_PLACEMENT_3D('',#12922,#7715,#7716);
#6198=AXIS2_PLACEMENT_3D('',#12923,#7717,#7718);
#6199=AXIS2_PLACEMENT_3D('',#12924,#7719,#7720);
#6200=AXIS2_PLACEMENT_3D('',#12925,#7721,#7722);
#6201=AXIS2_PLACEMENT_3D('',#12926,#7723,#7724);
#6202=AXIS2_PLACEMENT_3D('',#12927,#7725,#7726);
#6203=AXIS2_PLACEMENT_3D('',#12928,#7727,#7728);
#6204=AXIS2_PLACEMENT_3D('',#12929,#7729,#7730);
#6205=AXIS2_PLACEMENT_3D('',#12930,#7731,#7732);
#6206=AXIS2_PLACEMENT_3D('',#12931,#7733,#7734);
#6207=AXIS2_PLACEMENT_3D('',#12932,#7735,#7736);
#6208=AXIS2_PLACEMENT_3D('',#12933,#7737,#7738);
#6209=AXIS2_PLACEMENT_3D('',#12934,#7739,#7740);
#6210=AXIS2_PLACEMENT_3D('',#12935,#7741,#7742);
#6211=AXIS2_PLACEMENT_3D('',#12936,#7743,#7744);
#6212=AXIS2_PLACEMENT_3D('',#12937,#7745,#7746);
#6213=AXIS2_PLACEMENT_3D('',#12938,#7747,#7748);
#6214=AXIS2_PLACEMENT_3D('',#12939,#7749,#7750);
#6215=AXIS2_PLACEMENT_3D('',#12940,#7751,#7752);
#6216=AXIS2_PLACEMENT_3D('',#12941,#7753,#7754);
#6217=AXIS2_PLACEMENT_3D('',#12942,#7755,#7756);
#6218=AXIS2_PLACEMENT_3D('',#12943,#7757,#7758);
#6219=AXIS2_PLACEMENT_3D('',#12944,#7759,#7760);
#6220=AXIS2_PLACEMENT_3D('',#12945,#7761,#7762);
#6221=AXIS2_PLACEMENT_3D('',#12946,#7763,#7764);
#6222=DIRECTION('axis',(0.,0.,1.));
#6223=DIRECTION('refdir',(1.,0.,0.));
#6224=DIRECTION('axis',(0.,0.,1.));
#6225=DIRECTION('refdir',(1.,0.,0.));
#6226=DIRECTION('center_axis',(0.,-1.,0.));
#6227=DIRECTION('ref_axis',(0.,0.,-1.));
#6228=DIRECTION('center_axis',(0.,1.,0.));
#6229=DIRECTION('ref_axis',(0.,0.,1.));
#6230=DIRECTION('',(0.,-1.,0.));
#6231=DIRECTION('center_axis',(-1.30104260698261E-16,1.,0.));
#6232=DIRECTION('ref_axis',(-1.,-1.30104260698261E-16,0.));
#6233=DIRECTION('center_axis',(0.,-1.,0.));
#6234=DIRECTION('ref_axis',(0.,0.,-1.));
#6235=DIRECTION('center_axis',(0.,1.,0.));
#6236=DIRECTION('ref_axis',(0.,0.,1.));
#6237=DIRECTION('',(0.,-1.,0.));
#6238=DIRECTION('center_axis',(-1.30104260698261E-16,1.,0.));
#6239=DIRECTION('ref_axis',(-1.,-1.30104260698261E-16,0.));
#6240=DIRECTION('center_axis',(0.,-1.,0.));
#6241=DIRECTION('ref_axis',(0.,0.,-1.));
#6242=DIRECTION('center_axis',(0.,1.,0.));
#6243=DIRECTION('ref_axis',(0.,0.,1.));
#6244=DIRECTION('',(0.,-1.,0.));
#6245=DIRECTION('center_axis',(-1.30104260698261E-16,1.,0.));
#6246=DIRECTION('ref_axis',(-1.,-1.30104260698261E-16,0.));
#6247=DIRECTION('center_axis',(0.,-1.,0.));
#6248=DIRECTION('ref_axis',(0.,0.,-1.));
#6249=DIRECTION('center_axis',(0.,1.,0.));
#6250=DIRECTION('ref_axis',(0.,0.,1.));
#6251=DIRECTION('',(0.,-1.,0.));
#6252=DIRECTION('center_axis',(-1.30104260698261E-16,1.,0.));
#6253=DIRECTION('ref_axis',(-1.,-1.30104260698261E-16,0.));
#6254=DIRECTION('center_axis',(0.,-1.,0.));
#6255=DIRECTION('ref_axis',(0.,0.,-1.));
#6256=DIRECTION('center_axis',(0.,1.,0.));
#6257=DIRECTION('ref_axis',(0.,0.,1.));
#6258=DIRECTION('',(0.,-1.,0.));
#6259=DIRECTION('center_axis',(-1.30104260698261E-16,1.,0.));
#6260=DIRECTION('ref_axis',(-1.,-1.30104260698261E-16,0.));
#6261=DIRECTION('center_axis',(0.,-1.,0.));
#6262=DIRECTION('ref_axis',(0.,0.,-1.));
#6263=DIRECTION('center_axis',(0.,1.,0.));
#6264=DIRECTION('ref_axis',(0.,0.,1.));
#6265=DIRECTION('',(0.,-1.,0.));
#6266=DIRECTION('center_axis',(-1.30104260698261E-16,1.,0.));
#6267=DIRECTION('ref_axis',(-1.,-1.30104260698261E-16,0.));
#6268=DIRECTION('center_axis',(0.,-1.,0.));
#6269=DIRECTION('ref_axis',(0.,0.,-1.));
#6270=DIRECTION('center_axis',(0.,1.,0.));
#6271=DIRECTION('ref_axis',(0.,0.,1.));
#6272=DIRECTION('',(0.,-1.,0.));
#6273=DIRECTION('center_axis',(-1.30104260698261E-16,1.,0.));
#6274=DIRECTION('ref_axis',(-1.,-1.30104260698261E-16,0.));
#6275=DIRECTION('center_axis',(0.,-1.,0.));
#6276=DIRECTION('ref_axis',(0.,0.,-1.));
#6277=DIRECTION('center_axis',(0.,1.,0.));
#6278=DIRECTION('ref_axis',(0.,0.,1.));
#6279=DIRECTION('',(0.,-1.,0.));
#6280=DIRECTION('center_axis',(-1.30104260698261E-16,1.,0.));
#6281=DIRECTION('ref_axis',(-1.,-1.30104260698261E-16,0.));
#6282=DIRECTION('',(0.,-1.,0.));
#6283=DIRECTION('center_axis',(0.258819045102518,0.,0.965925826289069));
#6284=DIRECTION('ref_axis',(0.965925826289069,0.,-0.258819045102518));
#6285=DIRECTION('',(-0.965925826289069,-1.25671065518696E-16,0.258819045102518));
#6286=DIRECTION('',(0.,-1.,0.));
#6287=DIRECTION('',(-0.965925826289069,0.,0.258819045102518));
#6288=DIRECTION('center_axis',(0.,-1.,0.));
#6289=DIRECTION('ref_axis',(0.,0.,-1.));
#6290=DIRECTION('center_axis',(-1.30104260698261E-16,1.,0.));
#6291=DIRECTION('ref_axis',(-1.,-1.30104260698261E-16,0.));
#6292=DIRECTION('',(0.,-1.,0.));
#6293=DIRECTION('center_axis',(0.,1.,0.));
#6294=DIRECTION('ref_axis',(0.,0.,-1.));
#6295=DIRECTION('center_axis',(1.,0.,0.));
#6296=DIRECTION('ref_axis',(0.,0.,-1.));
#6297=DIRECTION('',(0.,0.,1.));
#6298=DIRECTION('',(0.,-1.,0.));
#6299=DIRECTION('',(0.,0.,1.));
#6300=DIRECTION('center_axis',(0.,-1.,0.));
#6301=DIRECTION('ref_axis',(0.,0.,-1.));
#6302=DIRECTION('center_axis',(-1.30104260698261E-16,1.,0.));
#6303=DIRECTION('ref_axis',(-1.,-1.30104260698261E-16,0.));
#6304=DIRECTION('',(0.,-1.,0.));
#6305=DIRECTION('center_axis',(0.,1.,0.));
#6306=DIRECTION('ref_axis',(0.,0.,1.));
#6307=DIRECTION('center_axis',(0.258819045102518,0.,-0.965925826289069));
#6308=DIRECTION('ref_axis',(-0.965925826289069,0.,-0.258819045102518));
#6309=DIRECTION('',(0.965925826289069,1.25671065518696E-16,0.258819045102518));
#6310=DIRECTION('',(0.,-1.,0.));
#6311=DIRECTION('',(0.965925826289069,0.,0.258819045102518));
#6312=DIRECTION('center_axis',(0.,-1.,0.));
#6313=DIRECTION('ref_axis',(0.608761429008724,0.,0.793353340291233));
#6314=DIRECTION('center_axis',(-1.30104260698261E-16,1.,0.));
#6315=DIRECTION('ref_axis',(-1.,-1.30104260698261E-16,0.));
#6316=DIRECTION('',(0.,-1.,0.));
#6317=DIRECTION('center_axis',(0.,1.,0.));
#6318=DIRECTION('ref_axis',(0.,0.,1.));
#6319=DIRECTION('center_axis',(-1.,0.,0.));
#6320=DIRECTION('ref_axis',(0.,0.,1.));
#6321=DIRECTION('',(0.,0.,1.));
#6322=DIRECTION('',(0.,0.,-1.));
#6323=DIRECTION('center_axis',(0.,1.,0.));
#6324=DIRECTION('ref_axis',(0.,0.,1.));
#6325=DIRECTION('center_axis',(-1.30104260698261E-16,1.,0.));
#6326=DIRECTION('ref_axis',(-1.,-1.30104260698261E-16,0.));
#6327=DIRECTION('center_axis',(0.,-1.,0.));
#6328=DIRECTION('ref_axis',(0.,0.,-1.));
#6329=DIRECTION('center_axis',(0.,-1.,0.));
#6330=DIRECTION('ref_axis',(0.,0.,-1.));
#6331=DIRECTION('',(0.,-1.,0.));
#6332=DIRECTION('center_axis',(0.,1.,0.));
#6333=DIRECTION('ref_axis',(0.,0.,1.));
#6334=DIRECTION('center_axis',(0.,-1.,0.));
#6335=DIRECTION('ref_axis',(0.,0.,-1.));
#6336=DIRECTION('center_axis',(0.,-1.,0.));
#6337=DIRECTION('ref_axis',(0.,0.,-1.));
#6338=DIRECTION('',(0.,-1.,0.));
#6339=DIRECTION('center_axis',(0.,1.,0.));
#6340=DIRECTION('ref_axis',(0.,0.,1.));
#6341=DIRECTION('center_axis',(0.,-1.,0.));
#6342=DIRECTION('ref_axis',(0.,0.,-1.));
#6343=DIRECTION('center_axis',(0.,-1.,0.));
#6344=DIRECTION('ref_axis',(0.,0.,-1.));
#6345=DIRECTION('',(0.,-1.,0.));
#6346=DIRECTION('center_axis',(0.,1.,0.));
#6347=DIRECTION('ref_axis',(0.,0.,1.));
#6348=DIRECTION('center_axis',(0.,-1.,0.));
#6349=DIRECTION('ref_axis',(0.,0.,-1.));
#6350=DIRECTION('center_axis',(0.,-1.,0.));
#6351=DIRECTION('ref_axis',(0.,0.,-1.));
#6352=DIRECTION('',(0.,-1.,0.));
#6353=DIRECTION('center_axis',(0.,1.,0.));
#6354=DIRECTION('ref_axis',(0.,0.,1.));
#6355=DIRECTION('center_axis',(0.,-1.,0.));
#6356=DIRECTION('ref_axis',(0.,0.,-1.));
#6357=DIRECTION('center_axis',(0.,-1.,0.));
#6358=DIRECTION('ref_axis',(0.,0.,-1.));
#6359=DIRECTION('',(0.,-1.,0.));
#6360=DIRECTION('center_axis',(0.,1.,0.));
#6361=DIRECTION('ref_axis',(0.,0.,1.));
#6362=DIRECTION('',(0.,-1.,0.));
#6363=DIRECTION('center_axis',(0.,-1.,0.));
#6364=DIRECTION('ref_axis',(0.,0.,-1.));
#6365=DIRECTION('center_axis',(0.,-1.,0.));
#6366=DIRECTION('ref_axis',(0.,0.,-1.));
#6367=DIRECTION('',(0.,-1.,0.));
#6368=DIRECTION('center_axis',(0.,1.,0.));
#6369=DIRECTION('ref_axis',(0.,0.,1.));
#6370=DIRECTION('center_axis',(0.,-1.,0.));
#6371=DIRECTION('ref_axis',(0.,0.,-1.));
#6372=DIRECTION('center_axis',(0.,-1.,0.));
#6373=DIRECTION('ref_axis',(0.,0.,-1.));
#6374=DIRECTION('',(0.,-1.,0.));
#6375=DIRECTION('center_axis',(0.,1.,0.));
#6376=DIRECTION('ref_axis',(0.,0.,1.));
#6377=DIRECTION('center_axis',(0.,-1.,0.));
#6378=DIRECTION('ref_axis',(0.,0.,-1.));
#6379=DIRECTION('center_axis',(0.,-1.,0.));
#6380=DIRECTION('ref_axis',(0.,0.,-1.));
#6381=DIRECTION('',(0.,-1.,0.));
#6382=DIRECTION('center_axis',(0.,1.,0.));
#6383=DIRECTION('ref_axis',(0.,0.,1.));
#6384=DIRECTION('center_axis',(-1.,0.,0.));
#6385=DIRECTION('ref_axis',(0.,0.,1.));
#6386=DIRECTION('',(0.,0.,1.));
#6387=DIRECTION('',(0.,-1.,0.));
#6388=DIRECTION('',(0.,0.,-1.));
#6389=DIRECTION('center_axis',(0.,-1.,0.));
#6390=DIRECTION('ref_axis',(0.608761429008723,0.,0.793353340291234));
#6391=DIRECTION('center_axis',(0.,-1.,0.));
#6392=DIRECTION('ref_axis',(0.,0.,-1.));
#6393=DIRECTION('',(0.,-1.,0.));
#6394=DIRECTION('center_axis',(0.,1.,0.));
#6395=DIRECTION('ref_axis',(0.,0.,1.));
#6396=DIRECTION('center_axis',(0.258819045102518,0.,-0.965925826289069));
#6397=DIRECTION('ref_axis',(-0.965925826289069,0.,-0.258819045102518));
#6398=DIRECTION('',(-0.965925826289069,0.,-0.258819045102518));
#6399=DIRECTION('',(0.,-1.,0.));
#6400=DIRECTION('',(0.965925826289069,0.,0.258819045102518));
#6401=DIRECTION('center_axis',(0.,-1.,0.));
#6402=DIRECTION('ref_axis',(0.,0.,-1.));
#6403=DIRECTION('center_axis',(0.,-1.,0.));
#6404=DIRECTION('ref_axis',(0.,0.,-1.));
#6405=DIRECTION('',(0.,-1.,0.));
#6406=DIRECTION('center_axis',(0.,1.,0.));
#6407=DIRECTION('ref_axis',(0.,0.,1.));
#6408=DIRECTION('center_axis',(1.,0.,0.));
#6409=DIRECTION('ref_axis',(0.,0.,-1.));
#6410=DIRECTION('',(0.,0.,1.));
#6411=DIRECTION('',(0.,-1.,0.));
#6412=DIRECTION('',(0.,0.,1.));
#6413=DIRECTION('center_axis',(0.,-1.,0.));
#6414=DIRECTION('ref_axis',(0.,0.,-1.));
#6415=DIRECTION('center_axis',(0.,-1.,0.));
#6416=DIRECTION('ref_axis',(0.,0.,-1.));
#6417=DIRECTION('',(0.,-1.,0.));
#6418=DIRECTION('center_axis',(0.,1.,0.));
#6419=DIRECTION('ref_axis',(0.,0.,-1.));
#6420=DIRECTION('center_axis',(0.258819045102518,0.,0.965925826289069));
#6421=DIRECTION('ref_axis',(0.965925826289069,0.,-0.258819045102518));
#6422=DIRECTION('',(0.965925826289069,0.,-0.258819045102518));
#6423=DIRECTION('',(-0.965925826289069,0.,0.258819045102518));
#6424=DIRECTION('center_axis',(0.,1.,0.));
#6425=DIRECTION('ref_axis',(0.,0.,1.));
#6426=DIRECTION('center_axis',(0.,-1.,0.));
#6427=DIRECTION('ref_axis',(0.,0.,-1.));
#6428=DIRECTION('center_axis',(0.499999999999999,0.,-0.866025403784439));
#6429=DIRECTION('ref_axis',(-0.866025403784439,0.,-0.499999999999999));
#6430=DIRECTION('',(0.866025403784439,0.,0.499999999999999));
#6431=DIRECTION('',(0.,-1.,0.));
#6432=DIRECTION('',(0.866025403784439,0.,0.499999999999999));
#6433=DIRECTION('',(0.,-1.,0.));
#6434=DIRECTION('center_axis',(-0.5,0.,-0.866025403784438));
#6435=DIRECTION('ref_axis',(-0.866025403784438,0.,0.5));
#6436=DIRECTION('',(0.866025403784438,0.,-0.5));
#6437=DIRECTION('',(0.,-1.,0.));
#6438=DIRECTION('',(0.866025403784438,0.,-0.5));
#6439=DIRECTION('center_axis',(-1.,0.,0.));
#6440=DIRECTION('ref_axis',(0.,0.,1.));
#6441=DIRECTION('',(0.,0.,-1.));
#6442=DIRECTION('',(0.,-1.,0.));
#6443=DIRECTION('',(0.,0.,-1.));
#6444=DIRECTION('center_axis',(-0.5,0.,0.866025403784439));
#6445=DIRECTION('ref_axis',(0.866025403784439,0.,0.5));
#6446=DIRECTION('',(-0.866025403784439,0.,-0.5));
#6447=DIRECTION('',(0.,-1.,0.));
#6448=DIRECTION('',(-0.866025403784439,0.,-0.5));
#6449=DIRECTION('center_axis',(0.5,0.,0.866025403784438));
#6450=DIRECTION('ref_axis',(0.866025403784438,0.,-0.5));
#6451=DIRECTION('',(-0.866025403784438,0.,0.5));
#6452=DIRECTION('',(0.,-1.,0.));
#6453=DIRECTION('',(-0.866025403784438,0.,0.5));
#6454=DIRECTION('center_axis',(1.,0.,0.));
#6455=DIRECTION('ref_axis',(0.,0.,-1.));
#6456=DIRECTION('',(0.,0.,1.));
#6457=DIRECTION('',(0.,0.,1.));
#6458=DIRECTION('center_axis',(0.,1.,0.));
#6459=DIRECTION('ref_axis',(0.,0.,1.));
#6460=DIRECTION('center_axis',(0.,1.,0.));
#6461=DIRECTION('ref_axis',(0.,0.,1.));
#6462=DIRECTION('center_axis',(0.866025403784438,0.,-0.500000000000002));
#6463=DIRECTION('ref_axis',(-0.500000000000002,0.,-0.866025403784437));
#6464=DIRECTION('',(0.500000000000002,0.,0.866025403784437));
#6465=DIRECTION('',(0.,-1.,0.));
#6466=DIRECTION('',(0.500000000000002,0.,0.866025403784437));
#6467=DIRECTION('',(0.,-1.,0.));
#6468=DIRECTION('center_axis',(0.,0.,-1.));
#6469=DIRECTION('ref_axis',(-1.,0.,0.));
#6470=DIRECTION('',(1.,0.,0.));
#6471=DIRECTION('',(0.,-1.,0.));
#6472=DIRECTION('',(1.,0.,0.));
#6473=DIRECTION('center_axis',(-0.866025403784436,0.,-0.500000000000005));
#6474=DIRECTION('ref_axis',(-0.500000000000005,0.,0.866025403784436));
#6475=DIRECTION('',(0.500000000000004,0.,-0.866025403784436));
#6476=DIRECTION('',(0.,-1.,0.));
#6477=DIRECTION('',(0.500000000000004,0.,-0.866025403784436));
#6478=DIRECTION('center_axis',(-0.866025403784438,0.,0.500000000000002));
#6479=DIRECTION('ref_axis',(0.500000000000002,0.,0.866025403784437));
#6480=DIRECTION('',(-0.500000000000002,0.,-0.866025403784438));
#6481=DIRECTION('',(0.,-1.,0.));
#6482=DIRECTION('',(-0.500000000000002,0.,-0.866025403784438));
#6483=DIRECTION('center_axis',(0.,0.,1.));
#6484=DIRECTION('ref_axis',(1.,0.,0.));
#6485=DIRECTION('',(-1.,0.,0.));
#6486=DIRECTION('',(0.,-1.,0.));
#6487=DIRECTION('',(-1.,0.,0.));
#6488=DIRECTION('center_axis',(0.866025403784439,0.,0.5));
#6489=DIRECTION('ref_axis',(0.5,0.,-0.866025403784439));
#6490=DIRECTION('',(-0.5,0.,0.866025403784439));
#6491=DIRECTION('',(-0.5,0.,0.866025403784439));
#6492=DIRECTION('center_axis',(0.,1.,0.));
#6493=DIRECTION('ref_axis',(0.,0.,1.));
#6494=DIRECTION('center_axis',(0.,1.,0.));
#6495=DIRECTION('ref_axis',(0.,0.,1.));
#6496=DIRECTION('center_axis',(-0.5,0.,-0.866025403784439));
#6497=DIRECTION('ref_axis',(-0.866025403784439,0.,0.5));
#6498=DIRECTION('',(0.866025403784439,0.,-0.5));
#6499=DIRECTION('',(0.,-1.,0.));
#6500=DIRECTION('',(0.866025403784439,0.,-0.5));
#6501=DIRECTION('',(0.,-1.,0.));
#6502=DIRECTION('center_axis',(-1.,0.,0.));
#6503=DIRECTION('ref_axis',(0.,0.,1.));
#6504=DIRECTION('',(0.,0.,-1.));
#6505=DIRECTION('',(0.,-1.,0.));
#6506=DIRECTION('',(0.,0.,-1.));
#6507=DIRECTION('center_axis',(-0.5,0.,0.866025403784439));
#6508=DIRECTION('ref_axis',(0.866025403784439,0.,0.5));
#6509=DIRECTION('',(-0.866025403784439,0.,-0.5));
#6510=DIRECTION('',(0.,-1.,0.));
#6511=DIRECTION('',(-0.866025403784439,0.,-0.5));
#6512=DIRECTION('center_axis',(0.499999999999999,0.,0.866025403784439));
#6513=DIRECTION('ref_axis',(0.866025403784439,0.,-0.499999999999999));
#6514=DIRECTION('',(-0.866025403784439,0.,0.499999999999999));
#6515=DIRECTION('',(0.,-1.,0.));
#6516=DIRECTION('',(-0.866025403784439,0.,0.499999999999999));
#6517=DIRECTION('center_axis',(1.,0.,0.));
#6518=DIRECTION('ref_axis',(0.,0.,-1.));
#6519=DIRECTION('',(0.,0.,1.));
#6520=DIRECTION('',(0.,-1.,0.));
#6521=DIRECTION('',(0.,0.,1.));
#6522=DIRECTION('center_axis',(0.499999999999998,0.,-0.86602540378444));
#6523=DIRECTION('ref_axis',(-0.86602540378444,0.,-0.499999999999998));
#6524=DIRECTION('',(0.86602540378444,0.,0.499999999999998));
#6525=DIRECTION('',(0.86602540378444,0.,0.499999999999998));
#6526=DIRECTION('center_axis',(0.,1.,0.));
#6527=DIRECTION('ref_axis',(0.,0.,1.));
#6528=DIRECTION('center_axis',(0.,1.,0.));
#6529=DIRECTION('ref_axis',(0.,0.,1.));
#6530=DIRECTION('axis',(0.,0.,1.));
#6531=DIRECTION('refdir',(1.,0.,0.));
#6532=DIRECTION('center_axis',(0.,-1.,0.));
#6533=DIRECTION('ref_axis',(0.,0.,-1.));
#6534=DIRECTION('center_axis',(0.,-1.,0.));
#6535=DIRECTION('ref_axis',(0.,0.,-1.));
#6536=DIRECTION('',(0.,1.,0.));
#6537=DIRECTION('center_axis',(0.,-1.,0.));
#6538=DIRECTION('ref_axis',(0.,0.,-1.));
#6539=DIRECTION('center_axis',(0.,-1.,0.));
#6540=DIRECTION('ref_axis',(0.,0.,-1.));
#6541=DIRECTION('center_axis',(0.,1.,0.));
#6542=DIRECTION('ref_axis',(0.,0.,-1.));
#6543=DIRECTION('',(0.,-1.,0.));
#6544=DIRECTION('center_axis',(0.,1.,0.));
#6545=DIRECTION('ref_axis',(0.,0.,-1.));
#6546=DIRECTION('',(0.,-1.,0.));
#6547=DIRECTION('center_axis',(0.,1.,0.));
#6548=DIRECTION('ref_axis',(0.,0.,1.));
#6549=DIRECTION('center_axis',(0.,1.,0.));
#6550=DIRECTION('ref_axis',(0.,0.,1.));
#6551=DIRECTION('',(0.,-1.,0.));
#6552=DIRECTION('center_axis',(0.,1.,0.));
#6553=DIRECTION('ref_axis',(0.,0.,1.));
#6554=DIRECTION('center_axis',(0.,-1.,0.));
#6555=DIRECTION('ref_axis',(0.,0.,-1.));
#6556=DIRECTION('center_axis',(0.,1.,0.));
#6557=DIRECTION('ref_axis',(0.,0.,1.));
#6558=DIRECTION('',(0.,-1.,0.));
#6559=DIRECTION('center_axis',(0.,1.,0.));
#6560=DIRECTION('ref_axis',(0.,0.,1.));
#6561=DIRECTION('center_axis',(0.,-1.,0.));
#6562=DIRECTION('ref_axis',(0.,0.,-1.));
#6563=DIRECTION('center_axis',(0.,1.,0.));
#6564=DIRECTION('ref_axis',(0.,0.,1.));
#6565=DIRECTION('',(0.,-1.,0.));
#6566=DIRECTION('center_axis',(0.,1.,0.));
#6567=DIRECTION('ref_axis',(0.,0.,1.));
#6568=DIRECTION('center_axis',(0.,1.,0.));
#6569=DIRECTION('ref_axis',(0.,0.,1.));
#6570=DIRECTION('center_axis',(0.,1.,0.));
#6571=DIRECTION('ref_axis',(0.,0.,1.));
#6572=DIRECTION('center_axis',(0.,1.,0.));
#6573=DIRECTION('ref_axis',(0.,0.,1.));
#6574=DIRECTION('',(-0.500000000000001,0.,0.866025403784438));
#6575=DIRECTION('',(9.91270557701033E-17,0.,1.));
#6576=DIRECTION('center_axis',(0.,1.,0.));
#6577=DIRECTION('ref_axis',(0.,0.,1.));
#6578=DIRECTION('',(0.,0.,-1.));
#6579=DIRECTION('center_axis',(0.,-1.,0.));
#6580=DIRECTION('ref_axis',(0.,0.,1.));
#6581=DIRECTION('',(1.,0.,0.));
#6582=DIRECTION('',(0.707106781186576,0.,-0.707106781186519));
#6583=DIRECTION('',(-0.707106781186549,0.,-0.707106781186546));
#6584=DIRECTION('',(0.707106781186548,0.,-0.707106781186547));
#6585=DIRECTION('',(-0.707106781186548,0.,-0.707106781186547));
#6586=DIRECTION('',(0.707106781186546,0.,-0.707106781186549));
#6587=DIRECTION('center_axis',(0.,-1.,0.));
#6588=DIRECTION('ref_axis',(0.,0.,1.));
#6589=DIRECTION('',(-0.819152044289008,0.,-0.573576436351023));
#6590=DIRECTION('',(0.573576436351062,0.,-0.819152044288981));
#6591=DIRECTION('',(-0.819152044288987,0.,-0.573576436351053));
#6592=DIRECTION('',(0.573576436351036,0.,-0.819152044288999));
#6593=DIRECTION('',(-0.819152044288996,0.,-0.57357643635104));
#6594=DIRECTION('',(0.573576436351043,0.,-0.819152044288994));
#6595=DIRECTION('',(-0.173648177666936,0.,-0.984807753012207));
#6596=DIRECTION('',(-0.984807753012208,0.,0.173648177666932));
#6597=DIRECTION('center_axis',(0.,-1.,0.));
#6598=DIRECTION('ref_axis',(0.,0.,1.));
#6599=DIRECTION('',(1.,0.,0.));
#6600=DIRECTION('',(4.45418905079446E-17,0.,1.));
#6601=DIRECTION('',(-1.,0.,0.));
#6602=DIRECTION('',(0.,0.,-1.));
#6603=DIRECTION('center_axis',(0.,-1.,0.));
#6604=DIRECTION('ref_axis',(0.,0.,1.));
#6605=DIRECTION('',(8.19364478113207E-17,0.,-1.));
#6606=DIRECTION('',(1.,0.,0.));
#6607=DIRECTION('',(1.,0.,0.));
#6608=DIRECTION('',(7.41956747162227E-17,0.,1.));
#6609=DIRECTION('',(-0.866025403784438,0.,-0.5));
#6610=DIRECTION('center_axis',(0.,-1.,0.));
#6611=DIRECTION('ref_axis',(0.,0.,1.));
#6612=DIRECTION('',(-5.78241158658935E-16,0.,-1.));
#6613=DIRECTION('',(0.866025403784439,0.,0.499999999999999));
#6614=DIRECTION('',(-0.5,0.,0.866025403784439));
#6615=DIRECTION('',(-0.984807753012207,0.,0.173648177666934));
#6616=DIRECTION('',(-0.173648177666936,0.,-0.984807753012207));
#6617=DIRECTION('center_axis',(0.,-1.,0.));
#6618=DIRECTION('ref_axis',(0.,0.,1.));
#6619=DIRECTION('center_axis',(0.,1.,0.));
#6620=DIRECTION('ref_axis',(0.,0.,1.));
#6621=DIRECTION('',(-0.500000000000001,0.,0.866025403784438));
#6622=DIRECTION('',(-0.984807753012208,0.,0.173648177666932));
#6623=DIRECTION('',(-0.173648177666936,0.,-0.984807753012207));
#6624=DIRECTION('',(0.573576436351043,0.,-0.819152044288994));
#6625=DIRECTION('',(-0.819152044288996,0.,-0.57357643635104));
#6626=DIRECTION('',(0.573576436351036,0.,-0.819152044288999));
#6627=DIRECTION('',(-0.819152044288987,0.,-0.573576436351053));
#6628=DIRECTION('',(0.573576436351062,0.,-0.819152044288981));
#6629=DIRECTION('',(-0.819152044289008,0.,-0.573576436351023));
#6630=DIRECTION('center_axis',(0.,-1.,0.));
#6631=DIRECTION('ref_axis',(0.,0.,1.));
#6632=DIRECTION('',(0.707106781186546,0.,-0.707106781186549));
#6633=DIRECTION('',(-0.707106781186548,0.,-0.707106781186547));
#6634=DIRECTION('',(0.707106781186548,0.,-0.707106781186547));
#6635=DIRECTION('',(-0.707106781186549,0.,-0.707106781186546));
#6636=DIRECTION('',(0.707106781186576,0.,-0.707106781186519));
#6637=DIRECTION('',(1.,0.,0.));
#6638=DIRECTION('center_axis',(0.,-1.,0.));
#6639=DIRECTION('ref_axis',(0.,0.,1.));
#6640=DIRECTION('',(0.,0.,-1.));
#6641=DIRECTION('center_axis',(0.,1.,0.));
#6642=DIRECTION('ref_axis',(0.,0.,1.));
#6643=DIRECTION('',(9.91270557701033E-17,0.,1.));
#6644=DIRECTION('',(0.866025403784438,0.,0.5));
#6645=DIRECTION('',(-7.41956747162227E-17,0.,-1.));
#6646=DIRECTION('',(-1.,0.,0.));
#6647=DIRECTION('',(5.20417042793039E-15,0.,1.));
#6648=DIRECTION('center_axis',(0.,1.,0.));
#6649=DIRECTION('ref_axis',(0.,0.,-1.));
#6650=DIRECTION('',(0.984807753012207,0.,-0.173648177666934));
#6651=DIRECTION('',(0.5,0.,-0.866025403784439));
#6652=DIRECTION('',(-0.866025403784439,0.,-0.499999999999999));
#6653=DIRECTION('center_axis',(0.,1.,0.));
#6654=DIRECTION('ref_axis',(0.,0.,-1.));
#6655=DIRECTION('',(0.173648177666936,0.,0.984807753012207));
#6656=DIRECTION('',(-1.,0.,-4.33680868994201E-16));
#6657=DIRECTION('',(-8.19364478113207E-17,0.,1.));
#6658=DIRECTION('center_axis',(0.,1.,0.));
#6659=DIRECTION('ref_axis',(0.,0.,-1.));
#6660=DIRECTION('',(2.89120579329468E-16,0.,1.));
#6661=DIRECTION('',(1.,0.,0.));
#6662=DIRECTION('',(-4.45418905079446E-17,0.,-1.));
#6663=DIRECTION('',(-1.,0.,0.));
#6664=DIRECTION('center_axis',(0.866025403784438,0.,0.500000000000001));
#6665=DIRECTION('ref_axis',(0.500000000000001,0.,-0.866025403784438));
#6666=DIRECTION('',(0.,-1.,0.));
#6667=DIRECTION('',(0.,-1.,0.));
#6668=DIRECTION('center_axis',(1.,0.,-9.91270557701033E-17));
#6669=DIRECTION('ref_axis',(-9.91270557701033E-17,0.,-1.));
#6670=DIRECTION('',(0.,-1.,0.));
#6671=DIRECTION('center_axis',(0.,-1.,0.));
#6672=DIRECTION('ref_axis',(1.22464679914735E-16,0.,1.));
#6673=DIRECTION('',(0.,-1.,0.));
#6674=DIRECTION('center_axis',(-1.,0.,0.));
#6675=DIRECTION('ref_axis',(0.,0.,1.));
#6676=DIRECTION('',(0.,-1.,0.));
#6677=DIRECTION('center_axis',(0.,-1.,0.));
#6678=DIRECTION('ref_axis',(0.,0.,-1.));
#6679=DIRECTION('',(0.,-1.,0.));
#6680=DIRECTION('center_axis',(0.,0.,-1.));
#6681=DIRECTION('ref_axis',(-1.,0.,0.));
#6682=DIRECTION('',(0.,-1.,0.));
#6683=DIRECTION('center_axis',(-0.707106781186519,0.,-0.707106781186576));
#6684=DIRECTION('ref_axis',(-0.707106781186576,0.,0.707106781186519));
#6685=DIRECTION('',(0.,-1.,0.));
#6686=DIRECTION('center_axis',(-0.707106781186546,0.,0.707106781186549));
#6687=DIRECTION('ref_axis',(0.707106781186549,0.,0.707106781186546));
#6688=DIRECTION('',(0.,-1.,0.));
#6689=DIRECTION('center_axis',(-0.707106781186547,0.,-0.707106781186548));
#6690=DIRECTION('ref_axis',(-0.707106781186548,0.,0.707106781186547));
#6691=DIRECTION('',(0.,-1.,0.));
#6692=DIRECTION('center_axis',(-0.707106781186547,0.,0.707106781186548));
#6693=DIRECTION('ref_axis',(0.707106781186548,0.,0.707106781186547));
#6694=DIRECTION('',(0.,-1.,0.));
#6695=DIRECTION('center_axis',(-0.707106781186549,0.,-0.707106781186546));
#6696=DIRECTION('ref_axis',(-0.707106781186546,0.,0.707106781186549));
#6697=DIRECTION('',(0.,-1.,0.));
#6698=DIRECTION('center_axis',(0.,-1.,0.));
#6699=DIRECTION('ref_axis',(0.,0.,-1.));
#6700=DIRECTION('',(0.,-1.,0.));
#6701=DIRECTION('center_axis',(-0.573576436351023,0.,0.819152044289008));
#6702=DIRECTION('ref_axis',(0.819152044289008,0.,0.573576436351023));
#6703=DIRECTION('',(0.,-1.,0.));
#6704=DIRECTION('center_axis',(-0.819152044288981,0.,-0.573576436351062));
#6705=DIRECTION('ref_axis',(-0.573576436351062,0.,0.819152044288981));
#6706=DIRECTION('',(0.,-1.,0.));
#6707=DIRECTION('center_axis',(-0.573576436351053,0.,0.819152044288987));
#6708=DIRECTION('ref_axis',(0.819152044288987,0.,0.573576436351053));
#6709=DIRECTION('',(0.,-1.,0.));
#6710=DIRECTION('center_axis',(-0.819152044288999,0.,-0.573576436351036));
#6711=DIRECTION('ref_axis',(-0.573576436351036,0.,0.819152044288999));
#6712=DIRECTION('',(0.,-1.,0.));
#6713=DIRECTION('center_axis',(-0.57357643635104,0.,0.819152044288996));
#6714=DIRECTION('ref_axis',(0.819152044288996,0.,0.57357643635104));
#6715=DIRECTION('',(0.,-1.,0.));
#6716=DIRECTION('center_axis',(-0.819152044288994,0.,-0.573576436351043));
#6717=DIRECTION('ref_axis',(-0.573576436351043,0.,0.819152044288994));
#6718=DIRECTION('',(0.,-1.,0.));
#6719=DIRECTION('center_axis',(-0.984807753012207,0.,0.173648177666936));
#6720=DIRECTION('ref_axis',(0.173648177666936,0.,0.984807753012207));
#6721=DIRECTION('',(0.,-1.,0.));
#6722=DIRECTION('center_axis',(0.173648177666932,0.,0.984807753012208));
#6723=DIRECTION('ref_axis',(0.984807753012208,0.,-0.173648177666932));
#6724=DIRECTION('center_axis',(-0.5,0.,0.866025403784439));
#6725=DIRECTION('ref_axis',(0.866025403784439,0.,0.5));
#6726=DIRECTION('',(0.,1.,0.));
#6727=DIRECTION('',(0.866025403784439,0.,0.499999999999999));
#6728=DIRECTION('',(0.,1.,0.));
#6729=DIRECTION('center_axis',(-0.866025403784439,0.,-0.5));
#6730=DIRECTION('ref_axis',(-0.5,0.,0.866025403784439));
#6731=DIRECTION('',(-0.5,0.,0.866025403784439));
#6732=DIRECTION('',(0.,1.,0.));
#6733=DIRECTION('center_axis',(-0.173648177666935,0.,-0.984807753012207));
#6734=DIRECTION('ref_axis',(-0.984807753012207,0.,0.173648177666935));
#6735=DIRECTION('',(-0.984807753012207,0.,0.173648177666934));
#6736=DIRECTION('',(0.,1.,0.));
#6737=DIRECTION('center_axis',(0.984807753012207,0.,-0.173648177666936));
#6738=DIRECTION('ref_axis',(-0.173648177666936,0.,-0.984807753012207));
#6739=DIRECTION('',(-0.173648177666936,0.,-0.984807753012207));
#6740=DIRECTION('',(0.,1.,0.));
#6741=DIRECTION('center_axis',(0.,1.,0.));
#6742=DIRECTION('ref_axis',(0.,0.,1.));
#6743=DIRECTION('center_axis',(0.,-1.,0.));
#6744=DIRECTION('ref_axis',(0.,0.,1.));
#6745=DIRECTION('center_axis',(0.,1.,0.));
#6746=DIRECTION('ref_axis',(0.,0.,1.));
#6747=DIRECTION('center_axis',(0.,0.,1.));
#6748=DIRECTION('ref_axis',(1.,0.,0.));
#6749=DIRECTION('',(0.,1.,0.));
#6750=DIRECTION('',(1.,0.,0.));
#6751=DIRECTION('',(0.,1.,0.));
#6752=DIRECTION('center_axis',(-1.,0.,7.41956747162227E-17));
#6753=DIRECTION('ref_axis',(7.41956747162227E-17,0.,1.));
#6754=DIRECTION('',(7.41956747162227E-17,0.,1.));
#6755=DIRECTION('',(0.,1.,0.));
#6756=DIRECTION('center_axis',(0.5,0.,-0.866025403784438));
#6757=DIRECTION('ref_axis',(-0.866025403784438,0.,-0.5));
#6758=DIRECTION('',(-0.866025403784438,0.,-0.5));
#6759=DIRECTION('',(0.,1.,0.));
#6760=DIRECTION('center_axis',(0.,1.,0.));
#6761=DIRECTION('ref_axis',(0.,0.,1.));
#6762=DIRECTION('center_axis',(0.,-1.,0.));
#6763=DIRECTION('ref_axis',(0.,0.,1.));
#6764=DIRECTION('',(0.,1.,0.));
#6765=DIRECTION('center_axis',(1.,0.,-5.78241158658935E-16));
#6766=DIRECTION('ref_axis',(-5.78241158658935E-16,0.,-1.));
#6767=DIRECTION('',(-5.78241158658935E-16,0.,-1.));
#6768=DIRECTION('center_axis',(0.,1.,0.));
#6769=DIRECTION('ref_axis',(0.,0.,1.));
#6770=DIRECTION('center_axis',(0.,1.,0.));
#6771=DIRECTION('ref_axis',(1.22464679914735E-16,0.,-1.));
#6772=DIRECTION('',(0.,1.,0.));
#6773=DIRECTION('center_axis',(0.,-1.,0.));
#6774=DIRECTION('ref_axis',(0.,0.,1.));
#6775=DIRECTION('',(0.,1.,0.));
#6776=DIRECTION('center_axis',(0.,0.,1.));
#6777=DIRECTION('ref_axis',(1.,0.,0.));
#6778=DIRECTION('',(1.,0.,0.));
#6779=DIRECTION('',(0.,1.,0.));
#6780=DIRECTION('center_axis',(-1.,0.,4.45418905079446E-17));
#6781=DIRECTION('ref_axis',(4.45418905079446E-17,0.,1.));
#6782=DIRECTION('',(4.45418905079446E-17,0.,1.));
#6783=DIRECTION('',(0.,1.,0.));
#6784=DIRECTION('center_axis',(0.,0.,-1.));
#6785=DIRECTION('ref_axis',(-1.,0.,0.));
#6786=DIRECTION('',(-1.,0.,0.));
#6787=DIRECTION('',(0.,1.,0.));
#6788=DIRECTION('center_axis',(1.,0.,0.));
#6789=DIRECTION('ref_axis',(0.,0.,-1.));
#6790=DIRECTION('',(0.,0.,-1.));
#6791=DIRECTION('',(0.,1.,0.));
#6792=DIRECTION('center_axis',(0.,1.,0.));
#6793=DIRECTION('ref_axis',(0.,0.,1.));
#6794=DIRECTION('center_axis',(0.,-1.,0.));
#6795=DIRECTION('ref_axis',(0.,0.,1.));
#6796=DIRECTION('',(0.,1.,0.));
#6797=DIRECTION('center_axis',(1.,0.,8.19364478113207E-17));
#6798=DIRECTION('ref_axis',(8.19364478113207E-17,0.,-1.));
#6799=DIRECTION('',(8.19364478113207E-17,0.,-1.));
#6800=DIRECTION('',(0.,1.,0.));
#6801=DIRECTION('center_axis',(0.,0.,1.));
#6802=DIRECTION('ref_axis',(1.,0.,0.));
#6803=DIRECTION('',(1.,0.,0.));
#6804=DIRECTION('center_axis',(0.,1.,0.));
#6805=DIRECTION('ref_axis',(0.,0.,1.));
#6806=DIRECTION('center_axis',(-4.33680868994201E-16,0.,1.));
#6807=DIRECTION('ref_axis',(1.,0.,4.33680868994201E-16));
#6808=DIRECTION('',(-1.,0.,-4.33680868994201E-16));
#6809=DIRECTION('',(0.,-1.,0.));
#6810=DIRECTION('center_axis',(1.,0.,8.19364478113207E-17));
#6811=DIRECTION('ref_axis',(8.19364478113207E-17,0.,-1.));
#6812=DIRECTION('',(-8.19364478113207E-17,0.,1.));
#6813=DIRECTION('',(0.,-1.,0.));
#6814=DIRECTION('center_axis',(0.,-1.,0.));
#6815=DIRECTION('ref_axis',(0.,0.,-1.));
#6816=DIRECTION('center_axis',(0.,1.,0.));
#6817=DIRECTION('ref_axis',(0.,0.,-1.));
#6818=DIRECTION('',(0.,-1.,0.));
#6819=DIRECTION('center_axis',(1.,0.,-2.89120579329468E-16));
#6820=DIRECTION('ref_axis',(-2.89120579329468E-16,0.,-1.));
#6821=DIRECTION('',(2.89120579329468E-16,0.,1.));
#6822=DIRECTION('',(0.,-1.,0.));
#6823=DIRECTION('center_axis',(0.,0.,-1.));
#6824=DIRECTION('ref_axis',(-1.,0.,0.));
#6825=DIRECTION('',(1.,0.,0.));
#6826=DIRECTION('',(0.,-1.,0.));
#6827=DIRECTION('center_axis',(-1.,0.,4.45418905079446E-17));
#6828=DIRECTION('ref_axis',(4.45418905079446E-17,0.,1.));
#6829=DIRECTION('',(-4.45418905079446E-17,0.,-1.));
#6830=DIRECTION('',(0.,-1.,0.));
#6831=DIRECTION('center_axis',(0.,0.,1.));
#6832=DIRECTION('ref_axis',(1.,0.,0.));
#6833=DIRECTION('',(-1.,0.,0.));
#6834=DIRECTION('center_axis',(0.,-1.,0.));
#6835=DIRECTION('ref_axis',(0.,0.,-1.));
#6836=DIRECTION('center_axis',(-0.866025403784439,0.,-0.5));
#6837=DIRECTION('ref_axis',(-0.5,0.,0.866025403784439));
#6838=DIRECTION('',(0.,-1.,0.));
#6839=DIRECTION('',(0.5,0.,-0.866025403784439));
#6840=DIRECTION('',(0.,-1.,0.));
#6841=DIRECTION('center_axis',(-0.5,0.,0.866025403784439));
#6842=DIRECTION('ref_axis',(0.866025403784439,0.,0.5));
#6843=DIRECTION('',(-0.866025403784439,0.,-0.499999999999999));
#6844=DIRECTION('',(0.,-1.,0.));
#6845=DIRECTION('center_axis',(0.,-1.,0.));
#6846=DIRECTION('ref_axis',(0.,0.,-1.));
#6847=DIRECTION('center_axis',(0.,1.,0.));
#6848=DIRECTION('ref_axis',(0.,0.,-1.));
#6849=DIRECTION('',(0.,-1.,0.));
#6850=DIRECTION('center_axis',(0.984807753012207,0.,-0.173648177666936));
#6851=DIRECTION('ref_axis',(-0.173648177666936,0.,-0.984807753012207));
#6852=DIRECTION('',(0.173648177666936,0.,0.984807753012207));
#6853=DIRECTION('',(0.,-1.,0.));
#6854=DIRECTION('center_axis',(-0.173648177666935,0.,-0.984807753012207));
#6855=DIRECTION('ref_axis',(-0.984807753012207,0.,0.173648177666935));
#6856=DIRECTION('',(0.984807753012207,0.,-0.173648177666934));
#6857=DIRECTION('center_axis',(0.,-1.,0.));
#6858=DIRECTION('ref_axis',(0.,0.,-1.));
#6859=DIRECTION('center_axis',(-1.,0.,7.41956747162227E-17));
#6860=DIRECTION('ref_axis',(7.41956747162227E-17,0.,1.));
#6861=DIRECTION('',(0.,-1.,0.));
#6862=DIRECTION('',(-7.41956747162227E-17,0.,-1.));
#6863=DIRECTION('',(0.,-1.,0.));
#6864=DIRECTION('center_axis',(0.,0.,1.));
#6865=DIRECTION('ref_axis',(1.,0.,0.));
#6866=DIRECTION('',(-1.,0.,0.));
#6867=DIRECTION('',(0.,-1.,0.));
#6868=DIRECTION('center_axis',(1.,0.,-5.20417042793039E-15));
#6869=DIRECTION('ref_axis',(-5.20417042793039E-15,0.,-1.));
#6870=DIRECTION('',(5.20417042793039E-15,0.,1.));
#6871=DIRECTION('',(0.,-1.,0.));
#6872=DIRECTION('center_axis',(0.,-1.,0.));
#6873=DIRECTION('ref_axis',(0.,0.,-1.));
#6874=DIRECTION('center_axis',(0.,1.,0.));
#6875=DIRECTION('ref_axis',(0.,0.,-1.));
#6876=DIRECTION('',(0.,-1.,0.));
#6877=DIRECTION('center_axis',(0.5,0.,-0.866025403784438));
#6878=DIRECTION('ref_axis',(-0.866025403784438,0.,-0.5));
#6879=DIRECTION('',(0.866025403784438,0.,0.5));
#6880=DIRECTION('center_axis',(0.,-1.,0.));
#6881=DIRECTION('ref_axis',(0.,0.,-1.));
#6882=DIRECTION('axis',(0.,0.,1.));
#6883=DIRECTION('refdir',(1.,0.,0.));
#6884=DIRECTION('center_axis',(0.,0.,-1.));
#6885=DIRECTION('ref_axis',(-1.,0.,0.));
#6886=DIRECTION('center_axis',(0.,0.,-1.));
#6887=DIRECTION('ref_axis',(-1.,0.,0.));
#6888=DIRECTION('',(0.,0.,1.));
#6889=DIRECTION('center_axis',(0.,0.,-1.));
#6890=DIRECTION('ref_axis',(-1.,0.,0.));
#6891=DIRECTION('center_axis',(0.,0.,-1.));
#6892=DIRECTION('ref_axis',(-1.,0.,0.));
#6893=DIRECTION('center_axis',(0.,0.,-1.));
#6894=DIRECTION('ref_axis',(-1.,0.,0.));
#6895=DIRECTION('',(0.,0.,-1.));
#6896=DIRECTION('center_axis',(0.,0.,-1.));
#6897=DIRECTION('ref_axis',(-1.,0.,0.));
#6898=DIRECTION('center_axis',(0.,0.,1.));
#6899=DIRECTION('ref_axis',(1.,0.,0.));
#6900=DIRECTION('center_axis',(0.,0.,1.));
#6901=DIRECTION('ref_axis',(1.,0.,0.));
#6902=DIRECTION('',(0.,0.,-1.));
#6903=DIRECTION('center_axis',(0.,0.,1.));
#6904=DIRECTION('ref_axis',(1.,0.,0.));
#6905=DIRECTION('center_axis',(0.,0.,1.));
#6906=DIRECTION('ref_axis',(1.,0.,0.));
#6907=DIRECTION('center_axis',(0.,0.,1.));
#6908=DIRECTION('ref_axis',(1.,0.,0.));
#6909=DIRECTION('',(0.,0.,1.));
#6910=DIRECTION('center_axis',(0.,0.,1.));
#6911=DIRECTION('ref_axis',(1.,0.,0.));
#6912=DIRECTION('center_axis',(0.,0.,-1.));
#6913=DIRECTION('ref_axis',(-1.,0.,0.));
#6914=DIRECTION('center_axis',(0.,0.,1.));
#6915=DIRECTION('ref_axis',(1.,0.,0.));
#6916=DIRECTION('',(0.,0.,-1.));
#6917=DIRECTION('center_axis',(0.,0.,1.));
#6918=DIRECTION('ref_axis',(1.,0.,0.));
#6919=DIRECTION('center_axis',(0.,0.,-1.));
#6920=DIRECTION('ref_axis',(-1.,0.,0.));
#6921=DIRECTION('center_axis',(0.,0.,1.));
#6922=DIRECTION('ref_axis',(1.,0.,0.));
#6923=DIRECTION('',(0.,0.,-1.));
#6924=DIRECTION('center_axis',(0.,0.,1.));
#6925=DIRECTION('ref_axis',(1.,0.,0.));
#6926=DIRECTION('',(0.,0.,-1.));
#6927=DIRECTION('center_axis',(0.,0.,1.));
#6928=DIRECTION('ref_axis',(1.,0.,0.));
#6929=DIRECTION('center_axis',(0.,0.,1.));
#6930=DIRECTION('ref_axis',(1.,0.,0.));
#6931=DIRECTION('center_axis',(0.,0.,1.));
#6932=DIRECTION('ref_axis',(1.,0.,0.));
#6933=DIRECTION('center_axis',(0.,0.,1.));
#6934=DIRECTION('ref_axis',(1.,0.,0.));
#6935=DIRECTION('center_axis',(0.,0.,1.));
#6936=DIRECTION('ref_axis',(1.,0.,0.));
#6937=DIRECTION('center_axis',(0.,0.,1.));
#6938=DIRECTION('ref_axis',(1.,0.,0.));
#6939=DIRECTION('center_axis',(0.,0.,1.));
#6940=DIRECTION('ref_axis',(1.,0.,0.));
#6941=DIRECTION('center_axis',(0.,0.,1.));
#6942=DIRECTION('ref_axis',(1.,0.,0.));
#6943=DIRECTION('center_axis',(0.,0.,1.));
#6944=DIRECTION('ref_axis',(1.,0.,0.));
#6945=DIRECTION('center_axis',(0.,0.,1.));
#6946=DIRECTION('ref_axis',(1.,0.,0.));
#6947=DIRECTION('center_axis',(0.,0.,1.));
#6948=DIRECTION('ref_axis',(1.,0.,0.));
#6949=DIRECTION('center_axis',(0.,0.,1.));
#6950=DIRECTION('ref_axis',(1.,0.,0.));
#6951=DIRECTION('center_axis',(0.,0.,1.));
#6952=DIRECTION('ref_axis',(1.,0.,0.));
#6953=DIRECTION('center_axis',(0.,0.,1.));
#6954=DIRECTION('ref_axis',(1.,0.,0.));
#6955=DIRECTION('center_axis',(0.,0.,1.));
#6956=DIRECTION('ref_axis',(1.,0.,0.));
#6957=DIRECTION('center_axis',(0.,0.,1.));
#6958=DIRECTION('ref_axis',(1.,0.,0.));
#6959=DIRECTION('center_axis',(0.,0.,1.));
#6960=DIRECTION('ref_axis',(1.,0.,0.));
#6961=DIRECTION('center_axis',(0.,0.,1.));
#6962=DIRECTION('ref_axis',(1.,0.,0.));
#6963=DIRECTION('center_axis',(0.,0.,1.));
#6964=DIRECTION('ref_axis',(1.,0.,0.));
#6965=DIRECTION('center_axis',(0.,0.,1.));
#6966=DIRECTION('ref_axis',(1.,0.,0.));
#6967=DIRECTION('center_axis',(0.,0.,1.));
#6968=DIRECTION('ref_axis',(1.,0.,0.));
#6969=DIRECTION('center_axis',(0.,0.,1.));
#6970=DIRECTION('ref_axis',(1.,0.,0.));
#6971=DIRECTION('center_axis',(0.,0.,1.));
#6972=DIRECTION('ref_axis',(1.,0.,0.));
#6973=DIRECTION('center_axis',(0.,0.,1.));
#6974=DIRECTION('ref_axis',(1.,0.,0.));
#6975=DIRECTION('center_axis',(0.,0.,1.));
#6976=DIRECTION('ref_axis',(1.,0.,0.));
#6977=DIRECTION('center_axis',(0.,0.,1.));
#6978=DIRECTION('ref_axis',(1.,0.,0.));
#6979=DIRECTION('center_axis',(0.,0.,1.));
#6980=DIRECTION('ref_axis',(1.,0.,0.));
#6981=DIRECTION('center_axis',(0.,0.,1.));
#6982=DIRECTION('ref_axis',(1.,0.,0.));
#6983=DIRECTION('center_axis',(0.,0.,1.));
#6984=DIRECTION('ref_axis',(1.,0.,0.));
#6985=DIRECTION('center_axis',(0.,0.,1.));
#6986=DIRECTION('ref_axis',(1.,0.,0.));
#6987=DIRECTION('center_axis',(0.,0.,1.));
#6988=DIRECTION('ref_axis',(1.,0.,0.));
#6989=DIRECTION('center_axis',(0.,0.,1.));
#6990=DIRECTION('ref_axis',(1.,0.,0.));
#6991=DIRECTION('center_axis',(0.,0.,1.));
#6992=DIRECTION('ref_axis',(1.,0.,0.));
#6993=DIRECTION('center_axis',(0.,0.,1.));
#6994=DIRECTION('ref_axis',(1.,0.,0.));
#6995=DIRECTION('center_axis',(0.,0.,1.));
#6996=DIRECTION('ref_axis',(1.,0.,0.));
#6997=DIRECTION('center_axis',(0.,0.,1.));
#6998=DIRECTION('ref_axis',(1.,0.,0.));
#6999=DIRECTION('center_axis',(0.,0.,1.));
#7000=DIRECTION('ref_axis',(1.,0.,0.));
#7001=DIRECTION('center_axis',(0.,0.,1.));
#7002=DIRECTION('ref_axis',(1.,0.,0.));
#7003=DIRECTION('center_axis',(0.,0.,1.));
#7004=DIRECTION('ref_axis',(1.,0.,0.));
#7005=DIRECTION('center_axis',(0.,0.,1.));
#7006=DIRECTION('ref_axis',(1.,0.,0.));
#7007=DIRECTION('center_axis',(0.,0.,1.));
#7008=DIRECTION('ref_axis',(1.,0.,0.));
#7009=DIRECTION('center_axis',(0.,0.,1.));
#7010=DIRECTION('ref_axis',(1.,0.,0.));
#7011=DIRECTION('center_axis',(0.,0.,1.));
#7012=DIRECTION('ref_axis',(1.,0.,0.));
#7013=DIRECTION('center_axis',(0.,0.,1.));
#7014=DIRECTION('ref_axis',(1.,0.,0.));
#7015=DIRECTION('center_axis',(0.,0.,1.));
#7016=DIRECTION('ref_axis',(1.,0.,0.));
#7017=DIRECTION('center_axis',(0.,0.,1.));
#7018=DIRECTION('ref_axis',(1.,0.,0.));
#7019=DIRECTION('center_axis',(0.,0.,1.));
#7020=DIRECTION('ref_axis',(1.,0.,0.));
#7021=DIRECTION('center_axis',(0.,0.,1.));
#7022=DIRECTION('ref_axis',(1.,0.,0.));
#7023=DIRECTION('center_axis',(0.,0.,1.));
#7024=DIRECTION('ref_axis',(1.,0.,0.));
#7025=DIRECTION('center_axis',(0.,0.,1.));
#7026=DIRECTION('ref_axis',(1.,0.,0.));
#7027=DIRECTION('center_axis',(0.,0.,1.));
#7028=DIRECTION('ref_axis',(1.,0.,0.));
#7029=DIRECTION('center_axis',(0.,0.,1.));
#7030=DIRECTION('ref_axis',(1.,0.,0.));
#7031=DIRECTION('center_axis',(0.,0.,1.));
#7032=DIRECTION('ref_axis',(1.,0.,0.));
#7033=DIRECTION('center_axis',(0.,0.,1.));
#7034=DIRECTION('ref_axis',(1.,0.,0.));
#7035=DIRECTION('center_axis',(0.,0.,1.));
#7036=DIRECTION('ref_axis',(1.,0.,0.));
#7037=DIRECTION('center_axis',(0.,0.,1.));
#7038=DIRECTION('ref_axis',(1.,0.,0.));
#7039=DIRECTION('center_axis',(0.,0.,1.));
#7040=DIRECTION('ref_axis',(1.,0.,0.));
#7041=DIRECTION('center_axis',(0.,0.,1.));
#7042=DIRECTION('ref_axis',(1.,0.,0.));
#7043=DIRECTION('center_axis',(0.,0.,1.));
#7044=DIRECTION('ref_axis',(1.,0.,0.));
#7045=DIRECTION('center_axis',(0.,0.,1.));
#7046=DIRECTION('ref_axis',(1.,0.,0.));
#7047=DIRECTION('center_axis',(0.,0.,1.));
#7048=DIRECTION('ref_axis',(1.,0.,0.));
#7049=DIRECTION('center_axis',(0.,0.,1.));
#7050=DIRECTION('ref_axis',(1.,0.,0.));
#7051=DIRECTION('center_axis',(0.,0.,1.));
#7052=DIRECTION('ref_axis',(1.,0.,0.));
#7053=DIRECTION('center_axis',(0.,0.,1.));
#7054=DIRECTION('ref_axis',(1.,0.,0.));
#7055=DIRECTION('center_axis',(0.,0.,1.));
#7056=DIRECTION('ref_axis',(1.,0.,0.));
#7057=DIRECTION('center_axis',(0.,0.,1.));
#7058=DIRECTION('ref_axis',(1.,0.,0.));
#7059=DIRECTION('center_axis',(0.,0.,1.));
#7060=DIRECTION('ref_axis',(1.,0.,0.));
#7061=DIRECTION('center_axis',(0.,0.,1.));
#7062=DIRECTION('ref_axis',(1.,0.,0.));
#7063=DIRECTION('center_axis',(0.,0.,1.));
#7064=DIRECTION('ref_axis',(1.,0.,0.));
#7065=DIRECTION('center_axis',(0.,0.,1.));
#7066=DIRECTION('ref_axis',(1.,0.,0.));
#7067=DIRECTION('center_axis',(0.,0.,1.));
#7068=DIRECTION('ref_axis',(1.,0.,0.));
#7069=DIRECTION('center_axis',(0.,0.,1.));
#7070=DIRECTION('ref_axis',(1.,0.,0.));
#7071=DIRECTION('center_axis',(0.,0.,1.));
#7072=DIRECTION('ref_axis',(1.,0.,0.));
#7073=DIRECTION('center_axis',(0.,0.,1.));
#7074=DIRECTION('ref_axis',(1.,0.,0.));
#7075=DIRECTION('center_axis',(0.,0.,1.));
#7076=DIRECTION('ref_axis',(1.,0.,0.));
#7077=DIRECTION('center_axis',(0.,0.,1.));
#7078=DIRECTION('ref_axis',(1.,0.,0.));
#7079=DIRECTION('center_axis',(0.,0.,1.));
#7080=DIRECTION('ref_axis',(1.,0.,0.));
#7081=DIRECTION('center_axis',(0.,0.,1.));
#7082=DIRECTION('ref_axis',(1.,0.,0.));
#7083=DIRECTION('center_axis',(0.,0.,1.));
#7084=DIRECTION('ref_axis',(1.,0.,0.));
#7085=DIRECTION('center_axis',(0.,0.,1.));
#7086=DIRECTION('ref_axis',(1.,0.,0.));
#7087=DIRECTION('center_axis',(0.,0.,1.));
#7088=DIRECTION('ref_axis',(1.,0.,0.));
#7089=DIRECTION('center_axis',(0.,0.,1.));
#7090=DIRECTION('ref_axis',(1.,0.,0.));
#7091=DIRECTION('',(0.,0.,-1.));
#7092=DIRECTION('',(0.,0.,-1.));
#7093=DIRECTION('center_axis',(0.,0.,-1.));
#7094=DIRECTION('ref_axis',(-1.,0.,0.));
#7095=DIRECTION('',(0.,0.,-1.));
#7096=DIRECTION('',(0.,0.,-1.));
#7097=DIRECTION('center_axis',(0.,0.,-1.));
#7098=DIRECTION('ref_axis',(-1.,0.,0.));
#7099=DIRECTION('',(0.,0.,-1.));
#7100=DIRECTION('',(0.,0.,-1.));
#7101=DIRECTION('center_axis',(0.,0.,-1.));
#7102=DIRECTION('ref_axis',(-1.,0.,0.));
#7103=DIRECTION('',(0.,0.,-1.));
#7104=DIRECTION('',(0.,0.,-1.));
#7105=DIRECTION('center_axis',(0.,0.,-1.));
#7106=DIRECTION('ref_axis',(-1.,0.,0.));
#7107=DIRECTION('',(0.,0.,-1.));
#7108=DIRECTION('',(0.,0.,-1.));
#7109=DIRECTION('center_axis',(0.,0.,-1.));
#7110=DIRECTION('ref_axis',(-1.,0.,0.));
#7111=DIRECTION('',(0.,0.,-1.));
#7112=DIRECTION('',(0.,0.,-1.));
#7113=DIRECTION('center_axis',(0.,0.,-1.));
#7114=DIRECTION('ref_axis',(-1.,0.,0.));
#7115=DIRECTION('',(0.,0.,-1.));
#7116=DIRECTION('',(0.,0.,-1.));
#7117=DIRECTION('center_axis',(0.,0.,-1.));
#7118=DIRECTION('ref_axis',(-1.,0.,0.));
#7119=DIRECTION('',(0.,0.,-1.));
#7120=DIRECTION('',(0.,0.,-1.));
#7121=DIRECTION('center_axis',(0.,0.,-1.));
#7122=DIRECTION('ref_axis',(-1.,0.,0.));
#7123=DIRECTION('',(0.,0.,-1.));
#7124=DIRECTION('',(0.,0.,-1.));
#7125=DIRECTION('center_axis',(0.,0.,-1.));
#7126=DIRECTION('ref_axis',(-1.,0.,0.));
#7127=DIRECTION('',(0.,0.,-1.));
#7128=DIRECTION('',(0.,0.,-1.));
#7129=DIRECTION('center_axis',(0.,0.,-1.));
#7130=DIRECTION('ref_axis',(-1.,0.,0.));
#7131=DIRECTION('',(0.,0.,-1.));
#7132=DIRECTION('',(0.,0.,-1.));
#7133=DIRECTION('center_axis',(0.,0.,-1.));
#7134=DIRECTION('ref_axis',(-1.,0.,0.));
#7135=DIRECTION('',(0.,0.,-1.));
#7136=DIRECTION('',(0.,0.,-1.));
#7137=DIRECTION('center_axis',(0.,0.,-1.));
#7138=DIRECTION('ref_axis',(-1.,0.,0.));
#7139=DIRECTION('',(0.,0.,-1.));
#7140=DIRECTION('',(0.,0.,-1.));
#7141=DIRECTION('center_axis',(0.,0.,-1.));
#7142=DIRECTION('ref_axis',(-1.,0.,0.));
#7143=DIRECTION('',(0.,0.,-1.));
#7144=DIRECTION('',(0.,0.,-1.));
#7145=DIRECTION('center_axis',(0.,0.,-1.));
#7146=DIRECTION('ref_axis',(-1.,0.,0.));
#7147=DIRECTION('',(0.,0.,-1.));
#7148=DIRECTION('',(0.,0.,-1.));
#7149=DIRECTION('center_axis',(0.,0.,-1.));
#7150=DIRECTION('ref_axis',(-1.,0.,0.));
#7151=DIRECTION('',(0.,0.,-1.));
#7152=DIRECTION('',(0.,0.,-1.));
#7153=DIRECTION('center_axis',(0.,0.,-1.));
#7154=DIRECTION('ref_axis',(-1.,0.,0.));
#7155=DIRECTION('',(0.,0.,-1.));
#7156=DIRECTION('',(0.,0.,-1.));
#7157=DIRECTION('center_axis',(0.,0.,-1.));
#7158=DIRECTION('ref_axis',(-1.,0.,0.));
#7159=DIRECTION('',(0.,0.,-1.));
#7160=DIRECTION('',(0.,0.,-1.));
#7161=DIRECTION('center_axis',(0.,0.,-1.));
#7162=DIRECTION('ref_axis',(-1.,0.,0.));
#7163=DIRECTION('',(0.,0.,-1.));
#7164=DIRECTION('',(0.,0.,-1.));
#7165=DIRECTION('center_axis',(0.,0.,-1.));
#7166=DIRECTION('ref_axis',(-1.,0.,0.));
#7167=DIRECTION('',(0.,0.,-1.));
#7168=DIRECTION('',(0.,0.,-1.));
#7169=DIRECTION('center_axis',(0.,0.,-1.));
#7170=DIRECTION('ref_axis',(-1.,0.,0.));
#7171=DIRECTION('',(0.,0.,-1.));
#7172=DIRECTION('',(0.,0.,-1.));
#7173=DIRECTION('center_axis',(0.,0.,-1.));
#7174=DIRECTION('ref_axis',(-1.,0.,0.));
#7175=DIRECTION('',(0.,0.,-1.));
#7176=DIRECTION('',(0.,0.,-1.));
#7177=DIRECTION('center_axis',(0.,0.,-1.));
#7178=DIRECTION('ref_axis',(-1.,0.,0.));
#7179=DIRECTION('',(0.,0.,-1.));
#7180=DIRECTION('',(0.,0.,-1.));
#7181=DIRECTION('center_axis',(0.,0.,-1.));
#7182=DIRECTION('ref_axis',(-1.,0.,0.));
#7183=DIRECTION('',(0.,0.,-1.));
#7184=DIRECTION('',(0.,0.,-1.));
#7185=DIRECTION('center_axis',(0.,0.,-1.));
#7186=DIRECTION('ref_axis',(-1.,0.,0.));
#7187=DIRECTION('',(0.,0.,-1.));
#7188=DIRECTION('',(0.,0.,-1.));
#7189=DIRECTION('center_axis',(0.,0.,-1.));
#7190=DIRECTION('ref_axis',(-1.,0.,0.));
#7191=DIRECTION('',(0.,0.,-1.));
#7192=DIRECTION('',(0.,0.,-1.));
#7193=DIRECTION('center_axis',(0.,0.,-1.));
#7194=DIRECTION('ref_axis',(-1.,0.,0.));
#7195=DIRECTION('',(0.,0.,-1.));
#7196=DIRECTION('',(0.,0.,-1.));
#7197=DIRECTION('center_axis',(0.,0.,-1.));
#7198=DIRECTION('ref_axis',(-1.,0.,0.));
#7199=DIRECTION('',(0.,0.,-1.));
#7200=DIRECTION('',(0.,0.,-1.));
#7201=DIRECTION('center_axis',(0.,0.,-1.));
#7202=DIRECTION('ref_axis',(-1.,0.,0.));
#7203=DIRECTION('',(0.,0.,-1.));
#7204=DIRECTION('',(0.,0.,-1.));
#7205=DIRECTION('center_axis',(0.,0.,-1.));
#7206=DIRECTION('ref_axis',(-1.,0.,0.));
#7207=DIRECTION('',(0.,0.,-1.));
#7208=DIRECTION('',(0.,0.,-1.));
#7209=DIRECTION('center_axis',(0.,0.,-1.));
#7210=DIRECTION('ref_axis',(-1.,0.,0.));
#7211=DIRECTION('',(0.,0.,-1.));
#7212=DIRECTION('',(0.,0.,-1.));
#7213=DIRECTION('center_axis',(0.,0.,-1.));
#7214=DIRECTION('ref_axis',(-1.,0.,0.));
#7215=DIRECTION('',(0.,0.,-1.));
#7216=DIRECTION('',(0.,0.,-1.));
#7217=DIRECTION('center_axis',(0.,0.,-1.));
#7218=DIRECTION('ref_axis',(-1.,0.,0.));
#7219=DIRECTION('',(0.,0.,-1.));
#7220=DIRECTION('',(0.,0.,-1.));
#7221=DIRECTION('center_axis',(0.,0.,-1.));
#7222=DIRECTION('ref_axis',(-1.,0.,0.));
#7223=DIRECTION('',(0.,0.,-1.));
#7224=DIRECTION('',(0.,0.,-1.));
#7225=DIRECTION('center_axis',(0.,0.,-1.));
#7226=DIRECTION('ref_axis',(-1.,0.,0.));
#7227=DIRECTION('',(0.,0.,-1.));
#7228=DIRECTION('',(0.,0.,-1.));
#7229=DIRECTION('center_axis',(0.,0.,-1.));
#7230=DIRECTION('ref_axis',(-1.,0.,0.));
#7231=DIRECTION('',(0.,0.,-1.));
#7232=DIRECTION('',(0.,0.,-1.));
#7233=DIRECTION('center_axis',(0.,0.,-1.));
#7234=DIRECTION('ref_axis',(-1.,0.,0.));
#7235=DIRECTION('',(0.,0.,-1.));
#7236=DIRECTION('',(0.,0.,-1.));
#7237=DIRECTION('center_axis',(0.,0.,-1.));
#7238=DIRECTION('ref_axis',(1.,-3.21624529935327E-16,0.));
#7239=DIRECTION('',(0.,0.,-1.));
#7240=DIRECTION('',(0.,0.,-1.));
#7241=DIRECTION('center_axis',(0.,0.,-1.));
#7242=DIRECTION('ref_axis',(-1.,0.,0.));
#7243=DIRECTION('',(0.,0.,-1.));
#7244=DIRECTION('',(0.,0.,-1.));
#7245=DIRECTION('center_axis',(0.,0.,-1.));
#7246=DIRECTION('ref_axis',(-1.,0.,0.));
#7247=DIRECTION('center_axis',(0.,0.,1.));
#7248=DIRECTION('ref_axis',(1.,0.,0.));
#7249=DIRECTION('center_axis',(0.,0.,-1.));
#7250=DIRECTION('ref_axis',(-1.,0.,0.));
#7251=DIRECTION('axis',(0.,0.,1.));
#7252=DIRECTION('refdir',(1.,0.,0.));
#7253=DIRECTION('center_axis',(0.,-1.,0.));
#7254=DIRECTION('ref_axis',(0.,0.,-1.));
#7255=DIRECTION('center_axis',(0.,1.,0.));
#7256=DIRECTION('ref_axis',(0.,0.,1.));
#7257=DIRECTION('',(0.,-1.,0.));
#7258=DIRECTION('center_axis',(0.,1.,0.));
#7259=DIRECTION('ref_axis',(0.,0.,1.));
#7260=DIRECTION('center_axis',(0.,-1.,0.));
#7261=DIRECTION('ref_axis',(0.,0.,-1.));
#7262=DIRECTION('center_axis',(0.,1.,0.));
#7263=DIRECTION('ref_axis',(0.,0.,1.));
#7264=DIRECTION('',(0.,-1.,0.));
#7265=DIRECTION('center_axis',(0.,1.,0.));
#7266=DIRECTION('ref_axis',(0.,0.,1.));
#7267=DIRECTION('center_axis',(0.,1.,0.));
#7268=DIRECTION('ref_axis',(0.,0.,1.));
#7269=DIRECTION('center_axis',(0.,1.,0.));
#7270=DIRECTION('ref_axis',(0.,0.,1.));
#7271=DIRECTION('',(1.,0.,-1.90819582357449E-16));
#7272=DIRECTION('center_axis',(0.,1.,0.));
#7273=DIRECTION('ref_axis',(0.,0.,1.));
#7274=DIRECTION('',(-1.,0.,1.90819582357449E-16));
#7275=DIRECTION('center_axis',(0.,1.,0.));
#7276=DIRECTION('ref_axis',(0.,0.,1.));
#7277=DIRECTION('center_axis',(0.,1.,0.));
#7278=DIRECTION('ref_axis',(0.,0.,1.));
#7279=DIRECTION('',(-1.,0.,1.90819582357449E-16));
#7280=DIRECTION('center_axis',(0.,1.,0.));
#7281=DIRECTION('ref_axis',(0.,0.,1.));
#7282=DIRECTION('',(1.,0.,-1.90819582357449E-16));
#7283=DIRECTION('center_axis',(0.,-1.,0.));
#7284=DIRECTION('ref_axis',(0.,0.,-1.));
#7285=DIRECTION('',(0.,-1.,0.));
#7286=DIRECTION('',(0.,-1.,0.));
#7287=DIRECTION('center_axis',(-1.90819582357449E-16,0.,-1.));
#7288=DIRECTION('ref_axis',(-1.,0.,1.90819582357449E-16));
#7289=DIRECTION('',(0.,-1.,0.));
#7290=DIRECTION('center_axis',(0.,-1.,0.));
#7291=DIRECTION('ref_axis',(0.,0.,-1.));
#7292=DIRECTION('',(0.,-1.,0.));
#7293=DIRECTION('center_axis',(1.90819582357449E-16,0.,1.));
#7294=DIRECTION('ref_axis',(1.,0.,-1.90819582357449E-16));
#7295=DIRECTION('axis',(0.,0.,1.));
#7296=DIRECTION('refdir',(1.,0.,0.));
#7297=DIRECTION('center_axis',(-1.,0.,0.));
#7298=DIRECTION('ref_axis',(0.,0.,1.));
#7299=DIRECTION('',(-0.500000000000004,-1.0605752387249E-16,-0.866025403784436));
#7300=DIRECTION('center_axis',(-1.,0.,0.));
#7301=DIRECTION('ref_axis',(0.,0.,1.));
#7302=DIRECTION('center_axis',(-1.,0.,0.));
#7303=DIRECTION('ref_axis',(0.,0.,1.));
#7304=DIRECTION('center_axis',(-1.,0.,0.));
#7305=DIRECTION('ref_axis',(0.,0.,1.));
#7306=DIRECTION('center_axis',(-1.,0.,0.));
#7307=DIRECTION('ref_axis',(0.,0.,1.));
#7308=DIRECTION('center_axis',(-1.,0.,0.));
#7309=DIRECTION('ref_axis',(0.,0.,1.));
#7310=DIRECTION('center_axis',(-1.,0.,0.));
#7311=DIRECTION('ref_axis',(0.,0.,1.));
#7312=DIRECTION('center_axis',(-1.,0.,0.));
#7313=DIRECTION('ref_axis',(0.,0.,1.));
#7314=DIRECTION('center_axis',(-1.,0.,0.));
#7315=DIRECTION('ref_axis',(0.,0.,1.));
#7316=DIRECTION('center_axis',(0.,1.,-1.22464679914735E-16));
#7317=DIRECTION('ref_axis',(0.,-1.22464679914735E-16,-1.));
#7318=DIRECTION('center_axis',(1.,0.,0.));
#7319=DIRECTION('ref_axis',(0.,0.,1.));
#7320=DIRECTION('center_axis',(-1.,0.,0.));
#7321=DIRECTION('ref_axis',(0.,0.,1.));
#7322=DIRECTION('center_axis',(-1.,0.,0.));
#7323=DIRECTION('ref_axis',(0.,0.,1.));
#7324=DIRECTION('',(0.707106781186544,8.65956056235497E-17,0.707106781186551));
#7325=DIRECTION('center_axis',(-1.,0.,0.));
#7326=DIRECTION('ref_axis',(0.,0.,1.));
#7327=DIRECTION('center_axis',(-1.,0.,0.));
#7328=DIRECTION('ref_axis',(0.,0.,1.));
#7329=DIRECTION('',(1.,0.,0.));
#7330=DIRECTION('center_axis',(-1.,0.,0.));
#7331=DIRECTION('ref_axis',(0.,0.,1.));
#7332=DIRECTION('center_axis',(-1.,0.,0.));
#7333=DIRECTION('ref_axis',(0.,0.,1.));
#7334=DIRECTION('',(1.,0.,0.));
#7335=DIRECTION('center_axis',(-1.,0.,0.));
#7336=DIRECTION('ref_axis',(0.,0.,1.));
#7337=DIRECTION('center_axis',(0.,6.12323399573677E-17,-1.));
#7338=DIRECTION('ref_axis',(0.,1.,0.));
#7339=DIRECTION('center_axis',(-1.,0.,0.));
#7340=DIRECTION('ref_axis',(0.,0.,1.));
#7341=DIRECTION('center_axis',(-1.,0.,0.));
#7342=DIRECTION('ref_axis',(0.,0.,1.));
#7343=DIRECTION('',(0.,-1.,1.50231459873716E-16));
#7344=DIRECTION('',(0.,-0.5,-0.866025403784438));
#7345=DIRECTION('',(0.,0.5,-0.866025403784438));
#7346=DIRECTION('',(0.,1.,0.));
#7347=DIRECTION('',(0.,0.5,0.866025403784438));
#7348=DIRECTION('',(0.,-0.5,0.866025403784438));
#7349=DIRECTION('center_axis',(-1.,0.,0.));
#7350=DIRECTION('ref_axis',(0.,0.,1.));
#7351=DIRECTION('center_axis',(-1.,0.,0.));
#7352=DIRECTION('ref_axis',(0.,0.,1.));
#7353=DIRECTION('center_axis',(0.,0.866025403784438,-0.5));
#7354=DIRECTION('ref_axis',(0.,0.5,0.866025403784438));
#7355=DIRECTION('',(0.,-0.5,-0.866025403784438));
#7356=DIRECTION('',(0.,-0.5,-0.866025403784438));
#7357=DIRECTION('',(-1.,0.,0.));
#7358=DIRECTION('',(-1.,0.,0.));
#7359=DIRECTION('center_axis',(0.,0.866025403784438,0.5));
#7360=DIRECTION('ref_axis',(0.,-0.5,0.866025403784438));
#7361=DIRECTION('',(0.,0.5,-0.866025403784438));
#7362=DIRECTION('',(0.,0.5,-0.866025403784438));
#7363=DIRECTION('',(-1.,0.,0.));
#7364=DIRECTION('center_axis',(0.,0.,1.));
#7365=DIRECTION('ref_axis',(1.,0.,0.));
#7366=DIRECTION('',(0.,1.,0.));
#7367=DIRECTION('',(0.,1.,0.));
#7368=DIRECTION('',(-1.,0.,0.));
#7369=DIRECTION('center_axis',(0.,-0.866025403784439,0.5));
#7370=DIRECTION('ref_axis',(0.,-0.5,-0.866025403784439));
#7371=DIRECTION('',(0.,0.5,0.866025403784438));
#7372=DIRECTION('',(0.,0.5,0.866025403784438));
#7373=DIRECTION('',(-1.,0.,0.));
#7374=DIRECTION('center_axis',(0.,-0.866025403784439,-0.5));
#7375=DIRECTION('ref_axis',(0.,0.5,-0.866025403784439));
#7376=DIRECTION('',(0.,-0.5,0.866025403784438));
#7377=DIRECTION('',(0.,-0.5,0.866025403784438));
#7378=DIRECTION('',(-1.,0.,0.));
#7379=DIRECTION('center_axis',(0.,-1.50231459873716E-16,-1.));
#7380=DIRECTION('ref_axis',(0.,1.,-1.50231459873716E-16));
#7381=DIRECTION('',(0.,-1.,1.50231459873716E-16));
#7382=DIRECTION('',(0.,-1.,1.50231459873716E-16));
#7383=DIRECTION('center_axis',(1.,0.,0.));
#7384=DIRECTION('ref_axis',(0.,0.,-1.));
#7385=DIRECTION('center_axis',(1.,0.,0.));
#7386=DIRECTION('ref_axis',(0.,0.,-1.));
#7387=DIRECTION('center_axis',(1.,0.,0.));
#7388=DIRECTION('ref_axis',(0.,0.,-1.));
#7389=DIRECTION('center_axis',(1.,0.,0.));
#7390=DIRECTION('ref_axis',(0.,0.,-1.));
#7391=DIRECTION('center_axis',(1.,0.,0.));
#7392=DIRECTION('ref_axis',(0.,0.,-1.));
#7393=DIRECTION('center_axis',(1.,0.,0.));
#7394=DIRECTION('ref_axis',(0.,0.,-1.));
#7395=DIRECTION('axis',(0.,0.,1.));
#7396=DIRECTION('refdir',(1.,0.,0.));
#7397=DIRECTION('center_axis',(-1.,-2.97906491917051E-43,0.));
#7398=DIRECTION('ref_axis',(0.,0.,1.));
#7399=DIRECTION('',(-0.500000000000004,-1.0605752387249E-16,-0.866025403784436));
#7400=DIRECTION('center_axis',(-1.,-2.97906491917051E-43,0.));
#7401=DIRECTION('ref_axis',(0.,0.,1.));
#7402=DIRECTION('center_axis',(-1.,-2.97906491917051E-43,0.));
#7403=DIRECTION('ref_axis',(0.,0.,1.));
#7404=DIRECTION('center_axis',(-1.,-2.97906491917051E-43,0.));
#7405=DIRECTION('ref_axis',(0.,0.,1.));
#7406=DIRECTION('center_axis',(-1.,-2.97906491917051E-43,0.));
#7407=DIRECTION('ref_axis',(0.,0.,1.));
#7408=DIRECTION('center_axis',(-1.,-2.97906491917051E-43,0.));
#7409=DIRECTION('ref_axis',(0.,0.,1.));
#7410=DIRECTION('center_axis',(-1.,-2.97906491917051E-43,0.));
#7411=DIRECTION('ref_axis',(0.,0.,1.));
#7412=DIRECTION('center_axis',(-1.,-2.97906491917051E-43,0.));
#7413=DIRECTION('ref_axis',(0.,0.,1.));
#7414=DIRECTION('center_axis',(-1.,-2.97906491917051E-43,0.));
#7415=DIRECTION('ref_axis',(0.,0.,1.));
#7416=DIRECTION('center_axis',(-2.97906491917051E-43,1.,-1.22464679914735E-16));
#7417=DIRECTION('ref_axis',(0.,-1.22464679914735E-16,-1.));
#7418=DIRECTION('center_axis',(1.,2.97906491917051E-43,0.));
#7419=DIRECTION('ref_axis',(0.,0.,1.));
#7420=DIRECTION('center_axis',(-1.,-2.97906491917051E-43,0.));
#7421=DIRECTION('ref_axis',(0.,0.,1.));
#7422=DIRECTION('center_axis',(-1.,-2.97906491917051E-43,0.));
#7423=DIRECTION('ref_axis',(0.,0.,1.));
#7424=DIRECTION('',(0.707106781186549,8.65956056235492E-17,0.707106781186547));
#7425=DIRECTION('center_axis',(-1.,-2.97906491917051E-43,0.));
#7426=DIRECTION('ref_axis',(0.,0.,1.));
#7427=DIRECTION('center_axis',(-1.,-2.97906491917051E-43,0.));
#7428=DIRECTION('ref_axis',(0.,0.,1.));
#7429=DIRECTION('',(1.,2.97906491917051E-43,0.));
#7430=DIRECTION('center_axis',(-1.,-2.97906491917051E-43,0.));
#7431=DIRECTION('ref_axis',(0.,0.,1.));
#7432=DIRECTION('center_axis',(-1.,-2.97906491917051E-43,0.));
#7433=DIRECTION('ref_axis',(0.,0.,1.));
#7434=DIRECTION('',(1.,2.97906491917051E-43,0.));
#7435=DIRECTION('center_axis',(-1.,-2.97906491917051E-43,0.));
#7436=DIRECTION('ref_axis',(0.,0.,1.));
#7437=DIRECTION('center_axis',(0.,6.12323399573677E-17,-1.));
#7438=DIRECTION('ref_axis',(0.,1.,0.));
#7439=DIRECTION('center_axis',(-1.,-2.97906491917051E-43,0.));
#7440=DIRECTION('ref_axis',(0.,0.,1.));
#7441=DIRECTION('center_axis',(-1.,-2.97906491917051E-43,0.));
#7442=DIRECTION('ref_axis',(0.,0.,1.));
#7443=DIRECTION('',(8.19972511286966E-38,-1.,1.50231459873716E-16));
#7444=DIRECTION('',(9.4039548065783E-38,-0.5,-0.866025403784438));
#7445=DIRECTION('',(0.,0.5,-0.866025403784438));
#7446=DIRECTION('',(2.97906491917051E-43,1.,0.));
#7447=DIRECTION('',(-9.4039548065783E-38,0.5,0.866025403784438));
#7448=DIRECTION('',(0.,-0.5,0.866025403784438));
#7449=DIRECTION('center_axis',(-1.,-2.97906491917051E-43,0.));
#7450=DIRECTION('ref_axis',(0.,0.,1.));
#7451=DIRECTION('center_axis',(-1.,-2.97906491917051E-43,0.));
#7452=DIRECTION('ref_axis',(0.,0.,1.));
#7453=DIRECTION('center_axis',(4.70197740328915E-38,0.866025403784438,-0.5));
#7454=DIRECTION('ref_axis',(-9.4039548065783E-38,0.5,0.866025403784438));
#7455=DIRECTION('',(9.4039548065783E-38,-0.5,-0.866025403784438));
#7456=DIRECTION('',(9.4039548065783E-38,-0.5,-0.866025403784438));
#7457=DIRECTION('',(-1.,-2.97906491917051E-43,0.));
#7458=DIRECTION('',(-1.,-2.97906491917051E-43,0.));
#7459=DIRECTION('center_axis',(9.4039548065783E-38,0.866025403784438,0.5));
#7460=DIRECTION('ref_axis',(-4.84544694858195E-54,-0.5,0.866025403784438));
#7461=DIRECTION('',(0.,0.5,-0.866025403784438));
#7462=DIRECTION('',(0.,0.5,-0.866025403784438));
#7463=DIRECTION('',(-1.,-2.97906491917051E-43,0.));
#7464=DIRECTION('center_axis',(0.,0.,1.));
#7465=DIRECTION('ref_axis',(1.,2.97906491917051E-43,0.));
#7466=DIRECTION('',(2.97906491917051E-43,1.,0.));
#7467=DIRECTION('',(2.97906491917051E-43,1.,0.));
#7468=DIRECTION('',(-1.,-2.97906491917051E-43,0.));
#7469=DIRECTION('center_axis',(-4.70197740328915E-38,-0.866025403784439,
0.5));
#7470=DIRECTION('ref_axis',(9.4039548065783E-38,-0.5,-0.866025403784439));
#7471=DIRECTION('',(-9.4039548065783E-38,0.5,0.866025403784438));
#7472=DIRECTION('',(-9.4039548065783E-38,0.5,0.866025403784438));
#7473=DIRECTION('',(-1.,-2.97906491917051E-43,0.));
#7474=DIRECTION('center_axis',(-4.70197740328915E-38,-0.866025403784439,
-0.5));
#7475=DIRECTION('ref_axis',(3.12210349931794E-54,0.5,-0.866025403784439));
#7476=DIRECTION('',(0.,-0.5,0.866025403784438));
#7477=DIRECTION('',(0.,-0.5,0.866025403784438));
#7478=DIRECTION('',(-1.,-2.97906491917051E-43,0.));
#7479=DIRECTION('center_axis',(0.,-1.50231459873716E-16,-1.));
#7480=DIRECTION('ref_axis',(-8.19972511286966E-38,1.,-1.50231459873716E-16));
#7481=DIRECTION('',(8.19972511286966E-38,-1.,1.50231459873716E-16));
#7482=DIRECTION('',(8.19972511286966E-38,-1.,1.50231459873716E-16));
#7483=DIRECTION('center_axis',(1.,2.97906491917051E-43,0.));
#7484=DIRECTION('ref_axis',(0.,0.,-1.));
#7485=DIRECTION('center_axis',(1.,2.97906491917051E-43,0.));
#7486=DIRECTION('ref_axis',(0.,0.,-1.));
#7487=DIRECTION('center_axis',(1.,2.97906491917051E-43,0.));
#7488=DIRECTION('ref_axis',(0.,0.,-1.));
#7489=DIRECTION('center_axis',(1.,2.97906491917051E-43,0.));
#7490=DIRECTION('ref_axis',(0.,0.,-1.));
#7491=DIRECTION('center_axis',(1.,2.97906491917051E-43,0.));
#7492=DIRECTION('ref_axis',(0.,0.,-1.));
#7493=DIRECTION('center_axis',(1.,2.97906491917051E-43,0.));
#7494=DIRECTION('ref_axis',(0.,0.,-1.));
#7495=DIRECTION('axis',(0.,0.,1.));
#7496=DIRECTION('refdir',(1.,0.,0.));
#7497=DIRECTION('center_axis',(-1.,0.,0.));
#7498=DIRECTION('ref_axis',(0.,0.,1.));
#7499=DIRECTION('',(-0.500000000000004,-1.0605752387249E-16,-0.866025403784436));
#7500=DIRECTION('center_axis',(-1.,0.,0.));
#7501=DIRECTION('ref_axis',(0.,0.,1.));
#7502=DIRECTION('center_axis',(-1.,0.,0.));
#7503=DIRECTION('ref_axis',(0.,0.,1.));
#7504=DIRECTION('center_axis',(-1.,0.,0.));
#7505=DIRECTION('ref_axis',(0.,0.,1.));
#7506=DIRECTION('center_axis',(-1.,0.,0.));
#7507=DIRECTION('ref_axis',(0.,0.,1.));
#7508=DIRECTION('center_axis',(-1.,0.,0.));
#7509=DIRECTION('ref_axis',(0.,0.,1.));
#7510=DIRECTION('center_axis',(-1.,0.,0.));
#7511=DIRECTION('ref_axis',(0.,0.,1.));
#7512=DIRECTION('center_axis',(-1.,0.,0.));
#7513=DIRECTION('ref_axis',(0.,0.,1.));
#7514=DIRECTION('center_axis',(-1.,0.,0.));
#7515=DIRECTION('ref_axis',(0.,0.,1.));
#7516=DIRECTION('center_axis',(0.,1.,-1.22464679914735E-16));
#7517=DIRECTION('ref_axis',(0.,-1.22464679914735E-16,-1.));
#7518=DIRECTION('center_axis',(1.,0.,0.));
#7519=DIRECTION('ref_axis',(0.,0.,1.));
#7520=DIRECTION('center_axis',(-1.,0.,0.));
#7521=DIRECTION('ref_axis',(0.,0.,1.));
#7522=DIRECTION('center_axis',(-1.,0.,0.));
#7523=DIRECTION('ref_axis',(0.,0.,1.));
#7524=DIRECTION('',(0.707106781186548,8.65956056235492E-17,0.707106781186547));
#7525=DIRECTION('center_axis',(-1.,0.,0.));
#7526=DIRECTION('ref_axis',(0.,0.,1.));
#7527=DIRECTION('center_axis',(-1.,0.,0.));
#7528=DIRECTION('ref_axis',(0.,0.,1.));
#7529=DIRECTION('',(1.,0.,0.));
#7530=DIRECTION('center_axis',(-1.,0.,0.));
#7531=DIRECTION('ref_axis',(0.,0.,1.));
#7532=DIRECTION('center_axis',(-1.,0.,0.));
#7533=DIRECTION('ref_axis',(0.,0.,1.));
#7534=DIRECTION('',(1.,0.,0.));
#7535=DIRECTION('center_axis',(-1.,0.,0.));
#7536=DIRECTION('ref_axis',(0.,0.,1.));
#7537=DIRECTION('center_axis',(0.,6.12323399573677E-17,-1.));
#7538=DIRECTION('ref_axis',(0.,1.,0.));
#7539=DIRECTION('center_axis',(-1.,0.,0.));
#7540=DIRECTION('ref_axis',(0.,0.,1.));
#7541=DIRECTION('center_axis',(-1.,0.,0.));
#7542=DIRECTION('ref_axis',(0.,0.,1.));
#7543=DIRECTION('',(0.,-1.,1.50231459873716E-16));
#7544=DIRECTION('',(0.,-0.5,-0.866025403784438));
#7545=DIRECTION('',(0.,0.5,-0.866025403784438));
#7546=DIRECTION('',(0.,1.,0.));
#7547=DIRECTION('',(0.,0.5,0.866025403784438));
#7548=DIRECTION('',(0.,-0.5,0.866025403784438));
#7549=DIRECTION('center_axis',(-1.,0.,0.));
#7550=DIRECTION('ref_axis',(0.,0.,1.));
#7551=DIRECTION('center_axis',(-1.,0.,0.));
#7552=DIRECTION('ref_axis',(0.,0.,1.));
#7553=DIRECTION('center_axis',(0.,0.866025403784438,-0.5));
#7554=DIRECTION('ref_axis',(0.,0.5,0.866025403784438));
#7555=DIRECTION('',(0.,-0.5,-0.866025403784438));
#7556=DIRECTION('',(0.,-0.5,-0.866025403784438));
#7557=DIRECTION('',(-1.,0.,0.));
#7558=DIRECTION('',(-1.,0.,0.));
#7559=DIRECTION('center_axis',(0.,0.866025403784438,0.5));
#7560=DIRECTION('ref_axis',(0.,-0.5,0.866025403784438));
#7561=DIRECTION('',(0.,0.5,-0.866025403784438));
#7562=DIRECTION('',(0.,0.5,-0.866025403784438));
#7563=DIRECTION('',(-1.,0.,0.));
#7564=DIRECTION('center_axis',(0.,0.,1.));
#7565=DIRECTION('ref_axis',(1.,0.,0.));
#7566=DIRECTION('',(0.,1.,0.));
#7567=DIRECTION('',(0.,1.,0.));
#7568=DIRECTION('',(-1.,0.,0.));
#7569=DIRECTION('center_axis',(0.,-0.866025403784439,0.5));
#7570=DIRECTION('ref_axis',(0.,-0.5,-0.866025403784439));
#7571=DIRECTION('',(0.,0.5,0.866025403784438));
#7572=DIRECTION('',(0.,0.5,0.866025403784438));
#7573=DIRECTION('',(-1.,0.,0.));
#7574=DIRECTION('center_axis',(0.,-0.866025403784439,-0.5));
#7575=DIRECTION('ref_axis',(0.,0.5,-0.866025403784439));
#7576=DIRECTION('',(0.,-0.5,0.866025403784438));
#7577=DIRECTION('',(0.,-0.5,0.866025403784438));
#7578=DIRECTION('',(-1.,0.,0.));
#7579=DIRECTION('center_axis',(0.,-1.50231459873716E-16,-1.));
#7580=DIRECTION('ref_axis',(0.,1.,-1.50231459873716E-16));
#7581=DIRECTION('',(0.,-1.,1.50231459873716E-16));
#7582=DIRECTION('',(0.,-1.,1.50231459873716E-16));
#7583=DIRECTION('center_axis',(1.,0.,0.));
#7584=DIRECTION('ref_axis',(0.,0.,-1.));
#7585=DIRECTION('center_axis',(1.,0.,0.));
#7586=DIRECTION('ref_axis',(0.,0.,-1.));
#7587=DIRECTION('center_axis',(1.,0.,0.));
#7588=DIRECTION('ref_axis',(0.,0.,-1.));
#7589=DIRECTION('center_axis',(1.,0.,0.));
#7590=DIRECTION('ref_axis',(0.,0.,-1.));
#7591=DIRECTION('center_axis',(1.,0.,0.));
#7592=DIRECTION('ref_axis',(0.,0.,-1.));
#7593=DIRECTION('center_axis',(1.,0.,0.));
#7594=DIRECTION('ref_axis',(0.,0.,-1.));
#7595=DIRECTION('axis',(0.,0.,1.));
#7596=DIRECTION('refdir',(1.,0.,0.));
#7597=DIRECTION('center_axis',(-1.,0.,0.));
#7598=DIRECTION('ref_axis',(0.,0.,1.));
#7599=DIRECTION('',(-0.500000000000004,-1.0605752387249E-16,-0.866025403784436));
#7600=DIRECTION('center_axis',(-1.,0.,0.));
#7601=DIRECTION('ref_axis',(0.,0.,1.));
#7602=DIRECTION('center_axis',(-1.,0.,0.));
#7603=DIRECTION('ref_axis',(0.,0.,1.));
#7604=DIRECTION('center_axis',(-1.,0.,0.));
#7605=DIRECTION('ref_axis',(0.,0.,1.));
#7606=DIRECTION('center_axis',(-1.,0.,0.));
#7607=DIRECTION('ref_axis',(0.,0.,1.));
#7608=DIRECTION('center_axis',(-1.,0.,0.));
#7609=DIRECTION('ref_axis',(0.,0.,1.));
#7610=DIRECTION('center_axis',(-1.,0.,0.));
#7611=DIRECTION('ref_axis',(0.,0.,1.));
#7612=DIRECTION('center_axis',(-1.,0.,0.));
#7613=DIRECTION('ref_axis',(0.,0.,1.));
#7614=DIRECTION('center_axis',(-1.,0.,0.));
#7615=DIRECTION('ref_axis',(0.,0.,1.));
#7616=DIRECTION('center_axis',(0.,1.,-1.22464679914735E-16));
#7617=DIRECTION('ref_axis',(0.,-1.22464679914735E-16,-1.));
#7618=DIRECTION('center_axis',(1.,0.,0.));
#7619=DIRECTION('ref_axis',(0.,0.,1.));
#7620=DIRECTION('center_axis',(-1.,0.,0.));
#7621=DIRECTION('ref_axis',(0.,0.,1.));
#7622=DIRECTION('center_axis',(-1.,0.,0.));
#7623=DIRECTION('ref_axis',(0.,0.,1.));
#7624=DIRECTION('',(0.707106781186549,8.65956056235491E-17,0.707106781186546));
#7625=DIRECTION('center_axis',(-1.,0.,0.));
#7626=DIRECTION('ref_axis',(0.,0.,1.));
#7627=DIRECTION('center_axis',(-1.,0.,0.));
#7628=DIRECTION('ref_axis',(0.,0.,1.));
#7629=DIRECTION('',(1.,0.,0.));
#7630=DIRECTION('center_axis',(-1.,0.,0.));
#7631=DIRECTION('ref_axis',(0.,0.,1.));
#7632=DIRECTION('center_axis',(-1.,0.,0.));
#7633=DIRECTION('ref_axis',(0.,0.,1.));
#7634=DIRECTION('',(1.,0.,0.));
#7635=DIRECTION('center_axis',(-1.,0.,0.));
#7636=DIRECTION('ref_axis',(0.,0.,1.));
#7637=DIRECTION('center_axis',(0.,6.12323399573677E-17,-1.));
#7638=DIRECTION('ref_axis',(0.,1.,0.));
#7639=DIRECTION('center_axis',(-1.,0.,0.));
#7640=DIRECTION('ref_axis',(0.,0.,1.));
#7641=DIRECTION('center_axis',(-1.,0.,0.));
#7642=DIRECTION('ref_axis',(0.,0.,1.));
#7643=DIRECTION('',(0.,-1.,-1.87789324842145E-16));
#7644=DIRECTION('',(0.,-0.5,-0.866025403784438));
#7645=DIRECTION('',(0.,0.5,-0.866025403784438));
#7646=DIRECTION('',(0.,1.,0.));
#7647=DIRECTION('',(0.,0.5,0.866025403784438));
#7648=DIRECTION('',(0.,-0.5,0.866025403784438));
#7649=DIRECTION('center_axis',(-1.,0.,0.));
#7650=DIRECTION('ref_axis',(0.,0.,1.));
#7651=DIRECTION('center_axis',(-1.,0.,0.));
#7652=DIRECTION('ref_axis',(0.,0.,1.));
#7653=DIRECTION('center_axis',(0.,0.866025403784438,-0.5));
#7654=DIRECTION('ref_axis',(0.,0.5,0.866025403784438));
#7655=DIRECTION('',(0.,-0.5,-0.866025403784438));
#7656=DIRECTION('',(0.,-0.5,-0.866025403784438));
#7657=DIRECTION('',(-1.,0.,0.));
#7658=DIRECTION('',(-1.,0.,0.));
#7659=DIRECTION('center_axis',(0.,0.866025403784438,0.5));
#7660=DIRECTION('ref_axis',(0.,-0.5,0.866025403784438));
#7661=DIRECTION('',(0.,0.5,-0.866025403784438));
#7662=DIRECTION('',(0.,0.5,-0.866025403784438));
#7663=DIRECTION('',(-1.,0.,0.));
#7664=DIRECTION('center_axis',(0.,0.,1.));
#7665=DIRECTION('ref_axis',(1.,0.,0.));
#7666=DIRECTION('',(0.,1.,0.));
#7667=DIRECTION('',(0.,1.,0.));
#7668=DIRECTION('',(-1.,0.,0.));
#7669=DIRECTION('center_axis',(0.,-0.866025403784438,0.5));
#7670=DIRECTION('ref_axis',(0.,-0.5,-0.866025403784438));
#7671=DIRECTION('',(0.,0.5,0.866025403784438));
#7672=DIRECTION('',(0.,0.5,0.866025403784438));
#7673=DIRECTION('',(-1.,0.,0.));
#7674=DIRECTION('center_axis',(0.,-0.866025403784439,-0.5));
#7675=DIRECTION('ref_axis',(0.,0.5,-0.866025403784439));
#7676=DIRECTION('',(0.,-0.5,0.866025403784438));
#7677=DIRECTION('',(0.,-0.5,0.866025403784438));
#7678=DIRECTION('',(-1.,0.,0.));
#7679=DIRECTION('center_axis',(0.,1.87789324842145E-16,-1.));
#7680=DIRECTION('ref_axis',(0.,1.,1.87789324842145E-16));
#7681=DIRECTION('',(0.,-1.,-1.87789324842145E-16));
#7682=DIRECTION('',(0.,-1.,-1.87789324842145E-16));
#7683=DIRECTION('center_axis',(1.,0.,0.));
#7684=DIRECTION('ref_axis',(0.,0.,-1.));
#7685=DIRECTION('center_axis',(1.,0.,0.));
#7686=DIRECTION('ref_axis',(0.,0.,-1.));
#7687=DIRECTION('center_axis',(1.,0.,0.));
#7688=DIRECTION('ref_axis',(0.,0.,-1.));
#7689=DIRECTION('center_axis',(1.,0.,0.));
#7690=DIRECTION('ref_axis',(0.,0.,-1.));
#7691=DIRECTION('center_axis',(1.,0.,0.));
#7692=DIRECTION('ref_axis',(0.,0.,-1.));
#7693=DIRECTION('center_axis',(1.,0.,0.));
#7694=DIRECTION('ref_axis',(0.,0.,-1.));
#7695=DIRECTION('',(0.,0.,1.));
#7696=DIRECTION('',(1.,0.,0.));
#7697=DIRECTION('',(-1.69964261199285E-15,1.,-3.91511440253739E-16));
#7698=DIRECTION('',(-0.709963595070542,-9.30966997318662E-16,0.704238378444765));
#7699=DIRECTION('',(-0.704238378444764,-2.34092171062173E-25,0.709963595070543));
#7700=DIRECTION('',(0.709963595070543,4.30041569038607E-25,0.704238378444764));
#7701=DIRECTION('',(0.98561487657606,-1.59416071995482E-22,0.169006849186528));
#7702=DIRECTION('',(0.169006849186528,8.76123873059982E-21,-0.98561487657606));
#7703=DIRECTION('',(0.,0.,1.));
#7704=DIRECTION('',(0.,-1.,0.));
#7705=DIRECTION('',(-5.45808109061281E-22,5.45808109061281E-22,1.));
#7706=DIRECTION('',(1.56720521980904E-21,-1.,5.45808109061281E-22));
#7707=DIRECTION('',(0.,0.,1.));
#7708=DIRECTION('',(0.,1.,0.));
#7709=DIRECTION('',(0.,0.,1.));
#7710=DIRECTION('',(0.,1.,0.));
#7711=DIRECTION('',(0.985614876576069,-2.25997078137874E-22,-0.169006849186476));
#7712=DIRECTION('',(0.169006849186476,-3.87455698980382E-21,0.985614876576069));
#7713=DIRECTION('',(0.704238378444765,1.120858601034E-25,0.709963595070542));
#7714=DIRECTION('',(0.709963595070542,6.45105099862873E-26,-0.704238378444765));
#7715=DIRECTION('',(-0.704238378444766,0.,0.70996359507054));
#7716=DIRECTION('',(0.70996359507054,0.,0.704238378444766));
#7717=DIRECTION('',(0.712834268932874,1.49995056424939E-21,0.701332521016198));
#7718=DIRECTION('',(0.701332521016198,7.10061263358089E-22,-0.712834268932874));
#7719=DIRECTION('',(-8.14007172941956E-16,1.,1.79884002581129E-16));
#7720=DIRECTION('',(-0.709963595070541,-4.5123424062919E-16,-0.704238378444766));
#7721=DIRECTION('',(0.712834268932872,0.,0.701332521016199));
#7722=DIRECTION('',(0.701332521016199,0.,-0.712834268932872));
#7723=DIRECTION('',(0.704238378444762,1.12085860103399E-25,0.709963595070545));
#7724=DIRECTION('',(0.709963595070545,6.45105099862875E-26,-0.704238378444762));
#7725=DIRECTION('',(-0.712834268932877,0.,0.701332521016195));
#7726=DIRECTION('',(0.701332521016195,0.,0.712834268932877));
#7727=DIRECTION('',(-0.712834268932877,-2.39315062119834E-25,0.701332521016195));
#7728=DIRECTION('',(0.701332521016195,4.27164375311417E-25,0.712834268932877));
#7729=DIRECTION('',(0.,0.,1.));
#7730=DIRECTION('',(0.,-1.,0.));
#7731=DIRECTION('',(0.,0.,1.));
#7732=DIRECTION('',(0.,-1.,0.));
#7733=DIRECTION('',(0.,0.,1.));
#7734=DIRECTION('',(0.,-1.,0.));
#7735=DIRECTION('',(-3.41461032501958E-26,3.41461032501958E-26,1.));
#7736=DIRECTION('',(1.24735277955503E-25,-1.,3.41461032501958E-26));
#7737=DIRECTION('',(0.,0.,1.));
#7738=DIRECTION('',(0.,-1.,0.));
#7739=DIRECTION('',(0.,0.,1.));
#7740=DIRECTION('',(0.,-1.,0.));
#7741=DIRECTION('',(0.,0.,1.));
#7742=DIRECTION('',(0.,1.,0.));
#7743=DIRECTION('',(0.,0.,1.));
#7744=DIRECTION('',(0.,1.,0.));
#7745=DIRECTION('',(0.,0.,1.));
#7746=DIRECTION('',(0.,1.,0.));
#7747=DIRECTION('',(0.,0.,1.));
#7748=DIRECTION('',(0.,1.,0.));
#7749=DIRECTION('',(3.41461032501958E-26,3.41461032501958E-26,1.));
#7750=DIRECTION('',(-1.24735277955504E-25,1.,-3.41461032501958E-26));
#7751=DIRECTION('',(1.36657969355633E-25,1.36657969355633E-25,1.));
#7752=DIRECTION('',(-4.70176245576281E-25,1.,-1.36657969355633E-25));
#7753=DIRECTION('',(1.36654857898421E-25,1.36654857898421E-25,1.));
#7754=DIRECTION('',(-4.70170549339865E-25,1.,-1.36654857898421E-25));
#7755=DIRECTION('',(0.,0.,1.));
#7756=DIRECTION('',(0.,1.,0.));
#7757=DIRECTION('',(0.,0.,1.));
#7758=DIRECTION('',(0.,1.,0.));
#7759=DIRECTION('',(0.,0.,1.));
#7760=DIRECTION('',(0.,-1.,0.));
#7761=DIRECTION('',(0.,0.,1.));
#7762=DIRECTION('',(0.,-1.,0.));
#7763=DIRECTION('',(0.,0.,1.));
#7764=DIRECTION('',(0.,-1.,0.));
#7765=CARTESIAN_POINT('',(0.,0.,0.));
#7766=CARTESIAN_POINT('',(0.,0.,0.));
#7767=CARTESIAN_POINT('Origin',(72.,22.,-30.));
#7768=CARTESIAN_POINT('',(72.,22.,-28.));
#7769=CARTESIAN_POINT('Origin',(72.,22.,-30.));
#7770=CARTESIAN_POINT('',(72.,19.,-28.));
#7771=CARTESIAN_POINT('',(72.,22.,-28.));
#7772=CARTESIAN_POINT('Origin',(72.,19.,-30.));
#7773=CARTESIAN_POINT('Origin',(72.,22.,30.));
#7774=CARTESIAN_POINT('',(72.,22.,32.));
#7775=CARTESIAN_POINT('Origin',(72.,22.,30.));
#7776=CARTESIAN_POINT('',(72.,19.,32.));
#7777=CARTESIAN_POINT('',(72.,22.,32.));
#7778=CARTESIAN_POINT('Origin',(72.,19.,30.));
#7779=CARTESIAN_POINT('Origin',(7.,22.,0.));
#7780=CARTESIAN_POINT('',(7.,22.,2.));
#7781=CARTESIAN_POINT('Origin',(7.,22.,0.));
#7782=CARTESIAN_POINT('',(7.,19.,2.));
#7783=CARTESIAN_POINT('',(7.,22.,2.));
#7784=CARTESIAN_POINT('Origin',(7.,19.,0.));
#7785=CARTESIAN_POINT('Origin',(42.,22.,18.));
#7786=CARTESIAN_POINT('',(42.,22.,20.5));
#7787=CARTESIAN_POINT('Origin',(42.,22.,18.));
#7788=CARTESIAN_POINT('',(42.,19.,20.5));
#7789=CARTESIAN_POINT('',(42.,22.,20.5));
#7790=CARTESIAN_POINT('Origin',(42.,19.,18.));
#7791=CARTESIAN_POINT('Origin',(42.,22.,-18.));
#7792=CARTESIAN_POINT('',(42.,22.,-15.5));
#7793=CARTESIAN_POINT('Origin',(42.,22.,-18.));
#7794=CARTESIAN_POINT('',(42.,19.,-15.5));
#7795=CARTESIAN_POINT('',(42.,22.,-15.5));
#7796=CARTESIAN_POINT('Origin',(42.,19.,-18.));
#7797=CARTESIAN_POINT('Origin',(12.,22.,12.5));
#7798=CARTESIAN_POINT('',(12.,22.,15.));
#7799=CARTESIAN_POINT('Origin',(12.,22.,12.5));
#7800=CARTESIAN_POINT('',(12.,19.,15.));
#7801=CARTESIAN_POINT('',(12.,22.,15.));
#7802=CARTESIAN_POINT('Origin',(12.,19.,12.5));
#7803=CARTESIAN_POINT('Origin',(12.,22.,-12.5));
#7804=CARTESIAN_POINT('',(12.,22.,-10.));
#7805=CARTESIAN_POINT('Origin',(12.,22.,-12.5));
#7806=CARTESIAN_POINT('',(12.,19.,-10.));
#7807=CARTESIAN_POINT('',(12.,22.,-10.));
#7808=CARTESIAN_POINT('Origin',(12.,19.,-12.5));
#7809=CARTESIAN_POINT('Origin',(72.,22.,-33.51013241176));
#7810=CARTESIAN_POINT('',(80.,22.,-33.51013241176));
#7811=CARTESIAN_POINT('',(69.9294476391799,22.,-41.2375390220725));
#7812=CARTESIAN_POINT('Origin',(72.,22.,-33.51013241176));
#7813=CARTESIAN_POINT('',(80.,19.,-33.51013241176));
#7814=CARTESIAN_POINT('',(80.,22.,-33.51013241176));
#7815=CARTESIAN_POINT('',(69.9294476391799,19.,-41.2375390220725));
#7816=CARTESIAN_POINT('Origin',(72.,19.,-33.51013241176));
#7817=CARTESIAN_POINT('',(69.9294476391799,22.,-41.2375390220725));
#7818=CARTESIAN_POINT('Origin',(69.9294476391799,22.,-41.2375390220725));
#7819=CARTESIAN_POINT('',(5.92944763917986,19.,-24.0887907064809));
#7820=CARTESIAN_POINT('',(69.9294476391799,19.,-41.2375390220725));
#7821=CARTESIAN_POINT('',(5.92944763917986,22.,-24.0887907064809));
#7822=CARTESIAN_POINT('',(5.92944763917986,22.,-24.0887907064809));
#7823=CARTESIAN_POINT('',(69.9294476391799,22.,-41.2375390220725));
#7824=CARTESIAN_POINT('Origin',(8.,22.,-16.3613840961683));
#7825=CARTESIAN_POINT('',(8.57252759403147E-16,19.,-16.3613840961683));
#7826=CARTESIAN_POINT('Origin',(8.,19.,-16.3613840961683));
#7827=CARTESIAN_POINT('',(3.46944695195361E-15,22.,-16.3613840961683));
#7828=CARTESIAN_POINT('',(3.46944695195361E-15,22.,-16.3613840961683));
#7829=CARTESIAN_POINT('Origin',(8.,22.,-16.3613840961683));
#7830=CARTESIAN_POINT('Origin',(3.46944695195361E-15,22.,-16.3613840961683));
#7831=CARTESIAN_POINT('',(3.46944695195361E-15,19.,16.3613840961683));
#7832=CARTESIAN_POINT('',(8.57252759403147E-16,19.,-50.));
#7833=CARTESIAN_POINT('',(3.46944695195361E-15,22.,16.3613840961683));
#7834=CARTESIAN_POINT('',(3.46944695195361E-15,22.,16.3613840961683));
#7835=CARTESIAN_POINT('',(3.46944695195361E-15,22.,-16.3613840961683));
#7836=CARTESIAN_POINT('Origin',(8.,22.,16.3613840961683));
#7837=CARTESIAN_POINT('',(5.92944763917986,19.,24.0887907064809));
#7838=CARTESIAN_POINT('Origin',(8.,19.,16.3613840961683));
#7839=CARTESIAN_POINT('',(5.92944763917986,22.,24.0887907064809));
#7840=CARTESIAN_POINT('',(5.92944763917986,22.,24.0887907064809));
#7841=CARTESIAN_POINT('Origin',(8.,22.,16.3613840961683));
#7842=CARTESIAN_POINT('Origin',(5.92944763917986,22.,24.0887907064809));
#7843=CARTESIAN_POINT('',(69.9294476391799,19.,41.2375390220725));
#7844=CARTESIAN_POINT('',(5.92944763917986,19.,24.0887907064809));
#7845=CARTESIAN_POINT('',(69.9294476391799,22.,41.2375390220725));
#7846=CARTESIAN_POINT('',(69.9294476391799,22.,41.2375390220725));
#7847=CARTESIAN_POINT('',(5.92944763917986,22.,24.0887907064809));
#7848=CARTESIAN_POINT('Origin',(72.,22.,33.51013241176));
#7849=CARTESIAN_POINT('',(80.,19.,33.5101324117599));
#7850=CARTESIAN_POINT('Origin',(72.,19.,33.51013241176));
#7851=CARTESIAN_POINT('',(80.,22.,33.51013241176));
#7852=CARTESIAN_POINT('',(80.,22.,33.51013241176));
#7853=CARTESIAN_POINT('Origin',(72.,22.,33.51013241176));
#7854=CARTESIAN_POINT('Origin',(80.,22.,33.51013241176));
#7855=CARTESIAN_POINT('',(80.,19.,-50.));
#7856=CARTESIAN_POINT('',(80.,22.,33.51013241176));
#7857=CARTESIAN_POINT('Origin',(72.,22.,-33.51013241176));
#7858=CARTESIAN_POINT('Origin',(8.57252759403147E-16,19.,-50.));
#7859=CARTESIAN_POINT('Origin',(72.,22.,-30.));
#7860=CARTESIAN_POINT('',(72.,3.,-28.));
#7861=CARTESIAN_POINT('Origin',(72.,3.,-30.));
#7862=CARTESIAN_POINT('',(72.,0.,-28.));
#7863=CARTESIAN_POINT('',(72.,22.,-28.));
#7864=CARTESIAN_POINT('Origin',(72.,0.,-30.));
#7865=CARTESIAN_POINT('Origin',(72.,22.,30.));
#7866=CARTESIAN_POINT('',(72.,3.,32.));
#7867=CARTESIAN_POINT('Origin',(72.,3.,30.));
#7868=CARTESIAN_POINT('',(72.,0.,32.));
#7869=CARTESIAN_POINT('',(72.,22.,32.));
#7870=CARTESIAN_POINT('Origin',(72.,0.,30.));
#7871=CARTESIAN_POINT('Origin',(42.,22.,18.));
#7872=CARTESIAN_POINT('',(42.,3.,20.5));
#7873=CARTESIAN_POINT('Origin',(42.,3.,18.));
#7874=CARTESIAN_POINT('',(42.,0.,20.5));
#7875=CARTESIAN_POINT('',(42.,22.,20.5));
#7876=CARTESIAN_POINT('Origin',(42.,0.,18.));
#7877=CARTESIAN_POINT('Origin',(12.,22.,12.5));
#7878=CARTESIAN_POINT('',(12.,3.,15.));
#7879=CARTESIAN_POINT('Origin',(12.,3.,12.5));
#7880=CARTESIAN_POINT('',(12.,0.,15.));
#7881=CARTESIAN_POINT('',(12.,22.,15.));
#7882=CARTESIAN_POINT('Origin',(12.,0.,12.5));
#7883=CARTESIAN_POINT('Origin',(72.,22.,-33.51013241176));
#7884=CARTESIAN_POINT('',(69.9294476391799,3.,-41.2375390220725));
#7885=CARTESIAN_POINT('',(80.,3.,-33.51013241176));
#7886=CARTESIAN_POINT('Origin',(72.,3.,-33.51013241176));
#7887=CARTESIAN_POINT('',(80.,0.,-33.51013241176));
#7888=CARTESIAN_POINT('',(80.,22.,-33.51013241176));
#7889=CARTESIAN_POINT('',(69.9294476391799,0.,-41.2375390220725));
#7890=CARTESIAN_POINT('Origin',(72.,0.,-33.51013241176));
#7891=CARTESIAN_POINT('',(69.9294476391799,22.,-41.2375390220725));
#7892=CARTESIAN_POINT('Origin',(12.,22.,-12.5));
#7893=CARTESIAN_POINT('',(12.,3.,-10.));
#7894=CARTESIAN_POINT('Origin',(12.,3.,-12.5));
#7895=CARTESIAN_POINT('',(12.,0.,-10.));
#7896=CARTESIAN_POINT('',(12.,22.,-10.));
#7897=CARTESIAN_POINT('Origin',(12.,0.,-12.5));
#7898=CARTESIAN_POINT('Origin',(42.,22.,-18.));
#7899=CARTESIAN_POINT('',(42.,3.,-15.5));
#7900=CARTESIAN_POINT('Origin',(42.,3.,-18.));
#7901=CARTESIAN_POINT('',(42.,0.,-15.5));
#7902=CARTESIAN_POINT('',(42.,22.,-15.5));
#7903=CARTESIAN_POINT('Origin',(42.,0.,-18.));
#7904=CARTESIAN_POINT('Origin',(7.,22.,0.));
#7905=CARTESIAN_POINT('',(7.,3.,2.));
#7906=CARTESIAN_POINT('Origin',(7.,3.,0.));
#7907=CARTESIAN_POINT('',(7.,0.,2.));
#7908=CARTESIAN_POINT('',(7.,22.,2.));
#7909=CARTESIAN_POINT('Origin',(7.,0.,0.));
#7910=CARTESIAN_POINT('Origin',(80.,22.,33.51013241176));
#7911=CARTESIAN_POINT('',(80.,3.,33.51013241176));
#7912=CARTESIAN_POINT('',(80.,3.,-50.));
#7913=CARTESIAN_POINT('',(80.,0.,33.51013241176));
#7914=CARTESIAN_POINT('',(80.,22.,33.51013241176));
#7915=CARTESIAN_POINT('',(80.,0.,33.51013241176));
#7916=CARTESIAN_POINT('Origin',(72.,22.,33.51013241176));
#7917=CARTESIAN_POINT('',(69.9294476391799,3.,41.2375390220725));
#7918=CARTESIAN_POINT('Origin',(72.,3.,33.51013241176));
#7919=CARTESIAN_POINT('',(69.9294476391799,0.,41.2375390220725));
#7920=CARTESIAN_POINT('',(69.9294476391799,22.,41.2375390220725));
#7921=CARTESIAN_POINT('Origin',(72.,0.,33.51013241176));
#7922=CARTESIAN_POINT('Origin',(5.92944763917986,22.,24.0887907064809));
#7923=CARTESIAN_POINT('',(5.92944763917986,3.,24.0887907064809));
#7924=CARTESIAN_POINT('',(5.92944763917986,3.,24.0887907064809));
#7925=CARTESIAN_POINT('',(5.92944763917986,0.,24.0887907064809));
#7926=CARTESIAN_POINT('',(5.92944763917986,22.,24.0887907064809));
#7927=CARTESIAN_POINT('',(5.92944763917986,0.,24.0887907064809));
#7928=CARTESIAN_POINT('Origin',(8.,22.,16.3613840961683));
#7929=CARTESIAN_POINT('',(5.20417042793042E-15,3.,16.3613840961683));
#7930=CARTESIAN_POINT('Origin',(8.,3.,16.3613840961683));
#7931=CARTESIAN_POINT('',(3.46944695195361E-15,0.,16.3613840961683));
#7932=CARTESIAN_POINT('',(3.46944695195361E-15,22.,16.3613840961683));
#7933=CARTESIAN_POINT('Origin',(8.,0.,16.3613840961683));
#7934=CARTESIAN_POINT('Origin',(3.46944695195361E-15,22.,-16.3613840961683));
#7935=CARTESIAN_POINT('',(1.83697019872103E-15,3.,-16.3613840961683));
#7936=CARTESIAN_POINT('',(1.83697019872103E-15,3.,-50.));
#7937=CARTESIAN_POINT('',(3.46944695195361E-15,0.,-16.3613840961683));
#7938=CARTESIAN_POINT('',(3.46944695195361E-15,22.,-16.3613840961683));
#7939=CARTESIAN_POINT('',(3.46944695195361E-15,0.,-16.3613840961683));
#7940=CARTESIAN_POINT('Origin',(8.,22.,-16.3613840961683));
#7941=CARTESIAN_POINT('',(5.92944763917986,3.,-24.0887907064809));
#7942=CARTESIAN_POINT('Origin',(8.,3.,-16.3613840961683));
#7943=CARTESIAN_POINT('',(5.92944763917986,0.,-24.0887907064809));
#7944=CARTESIAN_POINT('',(5.92944763917986,22.,-24.0887907064809));
#7945=CARTESIAN_POINT('Origin',(8.,0.,-16.3613840961683));
#7946=CARTESIAN_POINT('Origin',(69.9294476391799,22.,-41.2375390220725));
#7947=CARTESIAN_POINT('',(69.9294476391799,3.,-41.2375390220725));
#7948=CARTESIAN_POINT('',(69.9294476391799,0.,-41.2375390220725));
#7949=CARTESIAN_POINT('Origin',(72.,0.,-33.51013241176));
#7950=CARTESIAN_POINT('Origin',(1.83697019872103E-15,3.,-50.));
#7951=CARTESIAN_POINT('Origin',(5.,19.,1.15470053837925));
#7952=CARTESIAN_POINT('',(5.,3.,1.15470053837925));
#7953=CARTESIAN_POINT('',(7.00000000000001,3.,2.3094010767585));
#7954=CARTESIAN_POINT('',(5.,3.,1.15470053837925));
#7955=CARTESIAN_POINT('',(7.00000000000001,19.,2.3094010767585));
#7956=CARTESIAN_POINT('',(7.00000000000001,19.,2.3094010767585));
#7957=CARTESIAN_POINT('',(5.,19.,1.15470053837925));
#7958=CARTESIAN_POINT('',(5.,19.,1.15470053837925));
#7959=CARTESIAN_POINT('',(5.,19.,1.15470053837925));
#7960=CARTESIAN_POINT('Origin',(7.00000000000001,19.,2.3094010767585));
#7961=CARTESIAN_POINT('',(9.00000000000001,3.,1.15470053837925));
#7962=CARTESIAN_POINT('',(7.00000000000001,3.,2.3094010767585));
#7963=CARTESIAN_POINT('',(9.00000000000001,19.,1.15470053837925));
#7964=CARTESIAN_POINT('',(9.00000000000001,19.,1.15470053837925));
#7965=CARTESIAN_POINT('',(7.00000000000001,19.,2.3094010767585));
#7966=CARTESIAN_POINT('Origin',(9.00000000000001,19.,1.15470053837925));
#7967=CARTESIAN_POINT('',(9.00000000000001,3.,-1.15470053837925));
#7968=CARTESIAN_POINT('',(9.00000000000001,3.,1.15470053837925));
#7969=CARTESIAN_POINT('',(9.00000000000001,19.,-1.15470053837925));
#7970=CARTESIAN_POINT('',(9.00000000000001,19.,-1.15470053837925));
#7971=CARTESIAN_POINT('',(9.00000000000001,19.,1.15470053837925));
#7972=CARTESIAN_POINT('Origin',(9.00000000000001,19.,-1.15470053837925));
#7973=CARTESIAN_POINT('',(7.,3.,-2.30940107675851));
#7974=CARTESIAN_POINT('',(9.00000000000001,3.,-1.15470053837925));
#7975=CARTESIAN_POINT('',(7.,19.,-2.30940107675851));
#7976=CARTESIAN_POINT('',(7.,19.,-2.30940107675851));
#7977=CARTESIAN_POINT('',(9.00000000000001,19.,-1.15470053837925));
#7978=CARTESIAN_POINT('Origin',(7.,19.,-2.30940107675851));
#7979=CARTESIAN_POINT('',(5.,3.,-1.15470053837925));
#7980=CARTESIAN_POINT('',(7.,3.,-2.30940107675851));
#7981=CARTESIAN_POINT('',(5.,19.,-1.15470053837925));
#7982=CARTESIAN_POINT('',(5.,19.,-1.15470053837925));
#7983=CARTESIAN_POINT('',(7.,19.,-2.30940107675851));
#7984=CARTESIAN_POINT('Origin',(5.,19.,-1.15470053837925));
#7985=CARTESIAN_POINT('',(5.,3.,-1.15470053837925));
#7986=CARTESIAN_POINT('',(5.,19.,-1.15470053837925));
#7987=CARTESIAN_POINT('Origin',(7.00000000000001,19.,2.3094010767585));
#7988=CARTESIAN_POINT('Origin',(7.00000000000001,3.,2.3094010767585));
#7989=CARTESIAN_POINT('Origin',(69.6905989232415,19.,30.));
#7990=CARTESIAN_POINT('',(69.6905989232415,3.,30.));
#7991=CARTESIAN_POINT('',(70.8452994616208,3.,32.));
#7992=CARTESIAN_POINT('',(69.6905989232415,3.,30.));
#7993=CARTESIAN_POINT('',(70.8452994616208,19.,32.));
#7994=CARTESIAN_POINT('',(70.8452994616208,19.,32.));
#7995=CARTESIAN_POINT('',(69.6905989232415,19.,30.));
#7996=CARTESIAN_POINT('',(69.6905989232415,19.,30.));
#7997=CARTESIAN_POINT('',(69.6905989232415,19.,30.));
#7998=CARTESIAN_POINT('Origin',(70.8452994616208,19.,32.));
#7999=CARTESIAN_POINT('',(73.1547005383792,3.,32.));
#8000=CARTESIAN_POINT('',(70.8452994616208,3.,32.));
#8001=CARTESIAN_POINT('',(73.1547005383792,19.,32.));
#8002=CARTESIAN_POINT('',(73.1547005383792,19.,32.));
#8003=CARTESIAN_POINT('',(70.8452994616208,19.,32.));
#8004=CARTESIAN_POINT('Origin',(73.1547005383792,19.,32.));
#8005=CARTESIAN_POINT('',(74.3094010767585,3.,30.));
#8006=CARTESIAN_POINT('',(73.1547005383792,3.,32.));
#8007=CARTESIAN_POINT('',(74.3094010767585,19.,30.));
#8008=CARTESIAN_POINT('',(74.3094010767585,19.,30.));
#8009=CARTESIAN_POINT('',(73.1547005383792,19.,32.));
#8010=CARTESIAN_POINT('Origin',(74.3094010767585,19.,30.));
#8011=CARTESIAN_POINT('',(73.1547005383792,3.,28.));
#8012=CARTESIAN_POINT('',(74.3094010767585,3.,30.));
#8013=CARTESIAN_POINT('',(73.1547005383792,19.,28.));
#8014=CARTESIAN_POINT('',(73.1547005383792,19.,28.));
#8015=CARTESIAN_POINT('',(74.3094010767585,19.,30.));
#8016=CARTESIAN_POINT('Origin',(73.1547005383792,19.,28.));
#8017=CARTESIAN_POINT('',(70.8452994616208,3.,28.));
#8018=CARTESIAN_POINT('',(73.1547005383792,3.,28.));
#8019=CARTESIAN_POINT('',(70.8452994616208,19.,28.));
#8020=CARTESIAN_POINT('',(70.8452994616208,19.,28.));
#8021=CARTESIAN_POINT('',(73.1547005383792,19.,28.));
#8022=CARTESIAN_POINT('Origin',(70.8452994616208,19.,28.));
#8023=CARTESIAN_POINT('',(70.8452994616208,3.,28.));
#8024=CARTESIAN_POINT('',(70.8452994616208,19.,28.));
#8025=CARTESIAN_POINT('Origin',(70.8452994616208,19.,32.));
#8026=CARTESIAN_POINT('Origin',(70.8452994616208,3.,32.));
#8027=CARTESIAN_POINT('Origin',(72.0000000000001,19.,-27.6905989232415));
#8028=CARTESIAN_POINT('',(72.0000000000001,3.,-27.6905989232415));
#8029=CARTESIAN_POINT('',(74.,3.,-28.8452994616208));
#8030=CARTESIAN_POINT('',(72.0000000000001,3.,-27.6905989232415));
#8031=CARTESIAN_POINT('',(74.,19.,-28.8452994616208));
#8032=CARTESIAN_POINT('',(74.,19.,-28.8452994616208));
#8033=CARTESIAN_POINT('',(72.0000000000001,19.,-27.6905989232415));
#8034=CARTESIAN_POINT('',(72.0000000000001,19.,-27.6905989232415));
#8035=CARTESIAN_POINT('',(72.0000000000001,19.,-27.6905989232415));
#8036=CARTESIAN_POINT('Origin',(74.,19.,-28.8452994616208));
#8037=CARTESIAN_POINT('',(74.,3.,-31.1547005383792));
#8038=CARTESIAN_POINT('',(74.,3.,-28.8452994616208));
#8039=CARTESIAN_POINT('',(74.,19.,-31.1547005383792));
#8040=CARTESIAN_POINT('',(74.,19.,-31.1547005383792));
#8041=CARTESIAN_POINT('',(74.,19.,-28.8452994616208));
#8042=CARTESIAN_POINT('Origin',(74.,19.,-31.1547005383792));
#8043=CARTESIAN_POINT('',(72.,3.,-32.3094010767585));
#8044=CARTESIAN_POINT('',(74.,3.,-31.1547005383792));
#8045=CARTESIAN_POINT('',(72.,19.,-32.3094010767585));
#8046=CARTESIAN_POINT('',(72.,19.,-32.3094010767585));
#8047=CARTESIAN_POINT('',(74.,19.,-31.1547005383792));
#8048=CARTESIAN_POINT('Origin',(72.,19.,-32.3094010767585));
#8049=CARTESIAN_POINT('',(70.0000000000001,3.,-31.1547005383792));
#8050=CARTESIAN_POINT('',(72.,3.,-32.3094010767585));
#8051=CARTESIAN_POINT('',(70.0000000000001,19.,-31.1547005383792));
#8052=CARTESIAN_POINT('',(70.0000000000001,19.,-31.1547005383792));
#8053=CARTESIAN_POINT('',(72.,19.,-32.3094010767585));
#8054=CARTESIAN_POINT('Origin',(70.0000000000001,19.,-31.1547005383792));
#8055=CARTESIAN_POINT('',(70.0000000000001,3.,-28.8452994616208));
#8056=CARTESIAN_POINT('',(70.0000000000001,3.,-31.1547005383792));
#8057=CARTESIAN_POINT('',(70.0000000000001,19.,-28.8452994616208));
#8058=CARTESIAN_POINT('',(70.0000000000001,19.,-28.8452994616208));
#8059=CARTESIAN_POINT('',(70.0000000000001,19.,-31.1547005383792));
#8060=CARTESIAN_POINT('Origin',(70.0000000000001,19.,-28.8452994616208));
#8061=CARTESIAN_POINT('',(70.0000000000001,3.,-28.8452994616208));
#8062=CARTESIAN_POINT('',(70.0000000000001,19.,-28.8452994616208));
#8063=CARTESIAN_POINT('Origin',(74.,19.,-28.8452994616208));
#8064=CARTESIAN_POINT('Origin',(74.,3.,-28.8452994616208));
#8065=CARTESIAN_POINT('',(0.,0.,0.));
#8066=CARTESIAN_POINT('Origin',(0.,1.,-30.));
#8067=CARTESIAN_POINT('',(-4.28626379701573E-16,0.,-26.5));
#8068=CARTESIAN_POINT('Origin',(0.,0.,-30.));
#8069=CARTESIAN_POINT('',(-4.28626379701573E-16,1.,-26.5));
#8070=CARTESIAN_POINT('',(-4.28626379701573E-16,1.,-26.5));
#8071=CARTESIAN_POINT('Origin',(0.,1.,-30.));
#8072=CARTESIAN_POINT('Origin',(0.,1.,-7.86046575051991E-16));
#8073=CARTESIAN_POINT('',(3.50000000000001,1.,-2.82842712474618));
#8074=CARTESIAN_POINT('',(-3.50000000000001,1.,-2.82842712474618));
#8075=CARTESIAN_POINT('Origin',(0.,1.,-7.86046575051991E-16));
#8076=CARTESIAN_POINT('',(3.50000000000001,0.,-2.82842712474618));
#8077=CARTESIAN_POINT('',(3.50000000000001,1.,-2.82842712474618));
#8078=CARTESIAN_POINT('',(-3.50000000000001,0.,-2.82842712474618));
#8079=CARTESIAN_POINT('Origin',(0.,0.,-7.86046575051991E-16));
#8080=CARTESIAN_POINT('',(-3.50000000000001,1.,-2.82842712474618));
#8081=CARTESIAN_POINT('Origin',(0.,7.,-30.));
#8082=CARTESIAN_POINT('',(-4.28626379701574E-16,8.,-33.5));
#8083=CARTESIAN_POINT('Origin',(0.,8.,-30.));
#8084=CARTESIAN_POINT('',(-4.28626379701574E-16,7.,-33.5));
#8085=CARTESIAN_POINT('',(-4.28626379701574E-16,7.,-33.5));
#8086=CARTESIAN_POINT('Origin',(0.,7.,-30.));
#8087=CARTESIAN_POINT('Origin',(0.,8.,-30.));
#8088=CARTESIAN_POINT('',(-3.06161699786839E-16,8.,-27.5));
#8089=CARTESIAN_POINT('Origin',(0.,8.,-30.));
#8090=CARTESIAN_POINT('',(-3.06161699786839E-16,0.,-27.5));
#8091=CARTESIAN_POINT('',(-3.06161699786839E-16,8.,-27.5));
#8092=CARTESIAN_POINT('Origin',(0.,0.,-30.));
#8093=CARTESIAN_POINT('Origin',(0.,8.,-7.86046575051991E-16));
#8094=CARTESIAN_POINT('',(-3.06161699786838E-16,8.,2.5));
#8095=CARTESIAN_POINT('Origin',(0.,8.,-7.86046575051991E-16));
#8096=CARTESIAN_POINT('',(-3.06161699786838E-16,0.,2.5));
#8097=CARTESIAN_POINT('',(-3.06161699786838E-16,8.,2.5));
#8098=CARTESIAN_POINT('Origin',(0.,0.,-7.86046575051991E-16));
#8099=CARTESIAN_POINT('Origin',(0.,0.,-7.86046575051991E-16));
#8100=CARTESIAN_POINT('Origin',(0.,8.,-7.86046575051991E-16));
#8101=CARTESIAN_POINT('Origin',(0.,8.,-7.86046575051991E-16));
#8102=CARTESIAN_POINT('',(6.25000000000002,8.,-92.0836477965032));
#8103=CARTESIAN_POINT('',(-6.50000000000001,8.,-70.));
#8104=CARTESIAN_POINT('',(6.25000000000002,8.,-92.0836477965032));
#8105=CARTESIAN_POINT('',(-6.50000000000001,8.,0.));
#8106=CARTESIAN_POINT('',(-6.50000000000001,8.,-70.));
#8107=CARTESIAN_POINT('',(6.50000000000001,8.,-3.880363653291E-16));
#8108=CARTESIAN_POINT('Origin',(0.,8.,-7.86046575051991E-16));
#8109=CARTESIAN_POINT('',(6.50000000000001,8.,-24.));
#8110=CARTESIAN_POINT('',(6.50000000000001,8.,-7.86046575051991E-16));
#8111=CARTESIAN_POINT('',(16.5,8.,-34.));
#8112=CARTESIAN_POINT('Origin',(16.5,8.,-24.));
#8113=CARTESIAN_POINT('',(19.5,8.,-34.));
#8114=CARTESIAN_POINT('',(16.5,8.,-34.));
#8115=CARTESIAN_POINT('',(21.6213203435597,8.,-36.1213203435596));
#8116=CARTESIAN_POINT('',(19.5,8.,-34.));
#8117=CARTESIAN_POINT('',(19.6213203435597,8.,-38.1213203435595));
#8118=CARTESIAN_POINT('',(21.6213203435597,8.,-36.1213203435596));
#8119=CARTESIAN_POINT('',(21.6213203435597,8.,-40.1213203435595));
#8120=CARTESIAN_POINT('',(19.6213203435597,8.,-38.1213203435595));
#8121=CARTESIAN_POINT('',(19.6213203435597,8.,-42.1213203435595));
#8122=CARTESIAN_POINT('',(21.6213203435597,8.,-40.1213203435595));
#8123=CARTESIAN_POINT('',(21.6213203435597,8.,-44.1213203435596));
#8124=CARTESIAN_POINT('',(19.6213203435597,8.,-42.1213203435595));
#8125=CARTESIAN_POINT('',(13.5356539813314,8.,-79.5585032438718));
#8126=CARTESIAN_POINT('Origin',(31.3216319671078,8.,-64.9756713141856));
#8127=CARTESIAN_POINT('',(11.2187421199729,8.,-81.1808223945624));
#8128=CARTESIAN_POINT('',(13.5356539813313,8.,-79.5585032438719));
#8129=CARTESIAN_POINT('',(12.8410612706636,8.,-83.4977342559207));
#8130=CARTESIAN_POINT('',(11.2187421199729,8.,-81.1808223945624));
#8131=CARTESIAN_POINT('',(10.5241494093054,8.,-85.1200534066112));
#8132=CARTESIAN_POINT('',(12.8410612706636,8.,-83.4977342559207));
#8133=CARTESIAN_POINT('',(12.1464685599959,8.,-87.4369652679695));
#8134=CARTESIAN_POINT('',(10.5241494093054,8.,-85.1200534066112));
#8135=CARTESIAN_POINT('',(9.82955669863762,8.,-89.05928441866));
#8136=CARTESIAN_POINT('',(12.1464685599959,8.,-87.4369652679695));
#8137=CARTESIAN_POINT('',(11.4518758493282,8.,-91.3761962800183));
#8138=CARTESIAN_POINT('',(9.82955669863762,8.,-89.05928441866));
#8139=CARTESIAN_POINT('',(11.1740387650611,8.,-92.9518886848378));
#8140=CARTESIAN_POINT('',(11.4518758493282,8.,-91.3761962800183));
#8141=CARTESIAN_POINT('',(11.1740387650611,8.,-92.9518886848378));
#8142=CARTESIAN_POINT('',(-3.50000000000001,8.,-2.82842712474618));
#8143=CARTESIAN_POINT('',(3.50000000000001,8.,-2.82842712474618));
#8144=CARTESIAN_POINT('Origin',(0.,8.,-7.86046575051991E-16));
#8145=CARTESIAN_POINT('',(-4.50000000000001,8.,-2.82842712474618));
#8146=CARTESIAN_POINT('',(-4.50000000000001,8.,-2.82842712474618));
#8147=CARTESIAN_POINT('',(-4.50000000000001,8.,-41.7743150561845));
#8148=CARTESIAN_POINT('',(-4.50000000000001,8.,-2.82842712474618));
#8149=CARTESIAN_POINT('',(14.1836440347594,8.,-41.7743150561845));
#8150=CARTESIAN_POINT('',(-4.50000000000001,8.,-41.7743150561845));
#8151=CARTESIAN_POINT('',(14.1836440347594,8.,-35.7743150561845));
#8152=CARTESIAN_POINT('',(14.1836440347594,8.,-41.7743150561845));
#8153=CARTESIAN_POINT('',(4.50000000000001,8.,-24.));
#8154=CARTESIAN_POINT('Origin',(16.5,8.,-24.));
#8155=CARTESIAN_POINT('',(4.50000000000001,8.,-2.82842712474618));
#8156=CARTESIAN_POINT('',(4.50000000000001,8.,-2.82842712474618));
#8157=CARTESIAN_POINT('',(3.50000000000001,8.,-2.82842712474618));
#8158=CARTESIAN_POINT('',(-4.50000000000001,8.,-43.7743150561845));
#8159=CARTESIAN_POINT('',(14.1836440347594,8.,-43.7743150561845));
#8160=CARTESIAN_POINT('',(-4.50000000000001,8.,-43.7743150561845));
#8161=CARTESIAN_POINT('',(-4.50000000000001,8.,-67.1547005383792));
#8162=CARTESIAN_POINT('',(-4.50000000000001,8.,-67.1547005383792));
#8163=CARTESIAN_POINT('',(6.6910990889186,8.,-60.6935164668642));
#8164=CARTESIAN_POINT('',(-4.50000000000001,8.,-67.1547005383792));
#8165=CARTESIAN_POINT('',(14.1836440347593,8.,-46.7743150561846));
#8166=CARTESIAN_POINT('Origin',(31.3216319671078,8.,-64.9756713141856));
#8167=CARTESIAN_POINT('',(14.1836440347594,8.,-43.7743150561845));
#8168=CARTESIAN_POINT('',(-4.50000000000001,8.,-69.4641016151377));
#8169=CARTESIAN_POINT('',(6.38628307923174,8.,-63.1789031488688));
#8170=CARTESIAN_POINT('',(-4.50000000000001,8.,-69.4641016151377));
#8171=CARTESIAN_POINT('',(7.5157431494139,8.,-90.2759792406202));
#8172=CARTESIAN_POINT('',(7.5157431494139,8.,-90.2759792406202));
#8173=CARTESIAN_POINT('',(8.5669118613583,8.,-90.4613286458126));
#8174=CARTESIAN_POINT('',(7.5157431494139,8.,-90.2759792406202));
#8175=CARTESIAN_POINT('',(10.5956992404498,8.,-78.9555036669016));
#8176=CARTESIAN_POINT('',(8.5669118613583,8.,-90.4613286458126));
#8177=CARTESIAN_POINT('Origin',(31.3216319671078,8.,-64.9756713141856));
#8178=CARTESIAN_POINT('Origin',(0.,0.,-7.86046575051991E-16));
#8179=CARTESIAN_POINT('',(6.25000000000002,0.,-92.0836477965032));
#8180=CARTESIAN_POINT('',(-6.50000000000001,0.,-70.));
#8181=CARTESIAN_POINT('',(6.25000000000002,0.,-92.0836477965032));
#8182=CARTESIAN_POINT('',(11.1740387650611,0.,-92.9518886848378));
#8183=CARTESIAN_POINT('',(11.1740387650611,0.,-92.9518886848378));
#8184=CARTESIAN_POINT('',(11.4518758493282,0.,-91.3761962800183));
#8185=CARTESIAN_POINT('',(11.4518758493282,0.,-91.3761962800183));
#8186=CARTESIAN_POINT('',(9.82955669863762,0.,-89.05928441866));
#8187=CARTESIAN_POINT('',(9.82955669863762,0.,-89.05928441866));
#8188=CARTESIAN_POINT('',(12.1464685599959,0.,-87.4369652679695));
#8189=CARTESIAN_POINT('',(12.1464685599959,0.,-87.4369652679695));
#8190=CARTESIAN_POINT('',(10.5241494093054,0.,-85.1200534066112));
#8191=CARTESIAN_POINT('',(10.5241494093054,0.,-85.1200534066112));
#8192=CARTESIAN_POINT('',(12.8410612706636,0.,-83.4977342559207));
#8193=CARTESIAN_POINT('',(12.8410612706636,0.,-83.4977342559207));
#8194=CARTESIAN_POINT('',(11.2187421199729,0.,-81.1808223945624));
#8195=CARTESIAN_POINT('',(11.2187421199729,0.,-81.1808223945624));
#8196=CARTESIAN_POINT('',(13.5356539813314,0.,-79.5585032438718));
#8197=CARTESIAN_POINT('',(13.5356539813313,0.,-79.5585032438719));
#8198=CARTESIAN_POINT('',(21.6213203435597,0.,-44.1213203435596));
#8199=CARTESIAN_POINT('Origin',(31.3216319671078,0.,-64.9756713141856));
#8200=CARTESIAN_POINT('',(19.6213203435597,0.,-42.1213203435595));
#8201=CARTESIAN_POINT('',(19.6213203435597,0.,-42.1213203435595));
#8202=CARTESIAN_POINT('',(21.6213203435597,0.,-40.1213203435595));
#8203=CARTESIAN_POINT('',(21.6213203435597,0.,-40.1213203435595));
#8204=CARTESIAN_POINT('',(19.6213203435597,0.,-38.1213203435595));
#8205=CARTESIAN_POINT('',(19.6213203435597,0.,-38.1213203435595));
#8206=CARTESIAN_POINT('',(21.6213203435597,0.,-36.1213203435596));
#8207=CARTESIAN_POINT('',(21.6213203435597,0.,-36.1213203435596));
#8208=CARTESIAN_POINT('',(19.5,0.,-34.));
#8209=CARTESIAN_POINT('',(19.5,0.,-34.));
#8210=CARTESIAN_POINT('',(16.5,0.,-34.));
#8211=CARTESIAN_POINT('',(16.5,0.,-34.));
#8212=CARTESIAN_POINT('',(6.50000000000001,0.,-24.));
#8213=CARTESIAN_POINT('Origin',(16.5,0.,-24.));
#8214=CARTESIAN_POINT('',(6.50000000000001,0.,-3.880363653291E-16));
#8215=CARTESIAN_POINT('',(6.50000000000001,0.,-7.86046575051991E-16));
#8216=CARTESIAN_POINT('',(-6.50000000000001,0.,0.));
#8217=CARTESIAN_POINT('Origin',(0.,0.,-7.86046575051991E-16));
#8218=CARTESIAN_POINT('',(-6.50000000000001,0.,-70.));
#8219=CARTESIAN_POINT('',(-4.50000000000001,0.,-67.1547005383792));
#8220=CARTESIAN_POINT('',(6.6910990889186,0.,-60.6935164668642));
#8221=CARTESIAN_POINT('',(-4.50000000000001,0.,-67.1547005383792));
#8222=CARTESIAN_POINT('',(-4.50000000000001,0.,-43.7743150561845));
#8223=CARTESIAN_POINT('',(-4.50000000000001,0.,-43.7743150561845));
#8224=CARTESIAN_POINT('',(14.1836440347594,0.,-43.7743150561845));
#8225=CARTESIAN_POINT('',(14.1836440347594,0.,-43.7743150561845));
#8226=CARTESIAN_POINT('',(14.1836440347593,0.,-46.7743150561846));
#8227=CARTESIAN_POINT('',(14.1836440347593,0.,-46.7743150561846));
#8228=CARTESIAN_POINT('Origin',(31.3216319671078,0.,-64.9756713141856));
#8229=CARTESIAN_POINT('',(7.5157431494139,0.,-90.2759792406203));
#8230=CARTESIAN_POINT('',(8.5669118613583,0.,-90.4613286458126));
#8231=CARTESIAN_POINT('',(7.5157431494139,0.,-90.2759792406202));
#8232=CARTESIAN_POINT('',(-4.50000000000001,0.,-69.4641016151377));
#8233=CARTESIAN_POINT('',(-4.50000000000001,0.,-69.4641016151377));
#8234=CARTESIAN_POINT('',(6.38628307923175,0.,-63.1789031488688));
#8235=CARTESIAN_POINT('',(6.38628307923175,0.,-63.1789031488688));
#8236=CARTESIAN_POINT('',(10.5956992404498,0.,-78.9555036669016));
#8237=CARTESIAN_POINT('Origin',(31.3216319671078,0.,-64.9756713141856));
#8238=CARTESIAN_POINT('',(8.5669118613583,0.,-90.4613286458126));
#8239=CARTESIAN_POINT('',(4.50000000000001,0.,-2.82842712474618));
#8240=CARTESIAN_POINT('',(4.50000000000001,0.,-2.82842712474618));
#8241=CARTESIAN_POINT('',(4.50000000000001,0.,-24.));
#8242=CARTESIAN_POINT('',(4.50000000000001,0.,-24.));
#8243=CARTESIAN_POINT('',(14.1836440347594,0.,-35.7743150561845));
#8244=CARTESIAN_POINT('Origin',(16.5,0.,-24.));
#8245=CARTESIAN_POINT('',(14.1836440347594,0.,-41.7743150561845));
#8246=CARTESIAN_POINT('',(14.1836440347594,0.,-41.7743150561845));
#8247=CARTESIAN_POINT('',(-4.50000000000001,0.,-41.7743150561845));
#8248=CARTESIAN_POINT('',(-4.50000000000001,0.,-41.7743150561845));
#8249=CARTESIAN_POINT('',(-4.50000000000001,0.,-2.82842712474618));
#8250=CARTESIAN_POINT('',(-4.50000000000001,0.,-2.82842712474618));
#8251=CARTESIAN_POINT('',(-3.50000000000001,0.,-2.82842712474618));
#8252=CARTESIAN_POINT('Origin',(6.25000000000002,8.,-92.0836477965032));
#8253=CARTESIAN_POINT('',(-6.50000000000001,8.,-70.));
#8254=CARTESIAN_POINT('',(6.25000000000002,8.,-92.0836477965032));
#8255=CARTESIAN_POINT('Origin',(-6.50000000000001,8.,-70.));
#8256=CARTESIAN_POINT('',(-6.50000000000001,8.,0.));
#8257=CARTESIAN_POINT('Origin',(0.,8.,-7.86046575051991E-16));
#8258=CARTESIAN_POINT('',(6.50000000000001,8.,-3.880363653291E-16));
#8259=CARTESIAN_POINT('Origin',(6.50000000000001,8.,-7.86046575051991E-16));
#8260=CARTESIAN_POINT('',(6.50000000000001,8.,-24.));
#8261=CARTESIAN_POINT('Origin',(16.5,8.,-24.));
#8262=CARTESIAN_POINT('',(16.5,8.,-34.));
#8263=CARTESIAN_POINT('Origin',(16.5,8.,-34.));
#8264=CARTESIAN_POINT('',(19.5,8.,-34.));
#8265=CARTESIAN_POINT('Origin',(19.5,8.,-34.));
#8266=CARTESIAN_POINT('',(21.6213203435597,8.,-36.1213203435596));
#8267=CARTESIAN_POINT('Origin',(21.6213203435597,8.,-36.1213203435596));
#8268=CARTESIAN_POINT('',(19.6213203435597,8.,-38.1213203435595));
#8269=CARTESIAN_POINT('Origin',(19.6213203435597,8.,-38.1213203435595));
#8270=CARTESIAN_POINT('',(21.6213203435597,8.,-40.1213203435595));
#8271=CARTESIAN_POINT('Origin',(21.6213203435597,8.,-40.1213203435595));
#8272=CARTESIAN_POINT('',(19.6213203435597,8.,-42.1213203435595));
#8273=CARTESIAN_POINT('Origin',(19.6213203435597,8.,-42.1213203435595));
#8274=CARTESIAN_POINT('',(21.6213203435597,8.,-44.1213203435596));
#8275=CARTESIAN_POINT('Origin',(31.3216319671078,8.,-64.9756713141856));
#8276=CARTESIAN_POINT('',(13.5356539813314,8.,-79.5585032438718));
#8277=CARTESIAN_POINT('Origin',(13.5356539813313,8.,-79.5585032438719));
#8278=CARTESIAN_POINT('',(11.2187421199729,8.,-81.1808223945624));
#8279=CARTESIAN_POINT('Origin',(11.2187421199729,8.,-81.1808223945624));
#8280=CARTESIAN_POINT('',(12.8410612706636,8.,-83.4977342559207));
#8281=CARTESIAN_POINT('Origin',(12.8410612706636,8.,-83.4977342559207));
#8282=CARTESIAN_POINT('',(10.5241494093054,8.,-85.1200534066112));
#8283=CARTESIAN_POINT('Origin',(10.5241494093054,8.,-85.1200534066112));
#8284=CARTESIAN_POINT('',(12.1464685599959,8.,-87.4369652679695));
#8285=CARTESIAN_POINT('Origin',(12.1464685599959,8.,-87.4369652679695));
#8286=CARTESIAN_POINT('',(9.82955669863762,8.,-89.05928441866));
#8287=CARTESIAN_POINT('Origin',(9.82955669863762,8.,-89.05928441866));
#8288=CARTESIAN_POINT('',(11.4518758493282,8.,-91.3761962800183));
#8289=CARTESIAN_POINT('Origin',(11.4518758493282,8.,-91.3761962800183));
#8290=CARTESIAN_POINT('',(11.1740387650611,8.,-92.9518886848378));
#8291=CARTESIAN_POINT('Origin',(11.1740387650611,8.,-92.9518886848378));
#8292=CARTESIAN_POINT('Origin',(-4.50000000000001,7.,-69.4641016151377));
#8293=CARTESIAN_POINT('',(6.38628307923175,7.,-63.1789031488688));
#8294=CARTESIAN_POINT('',(6.38628307923175,7.,-63.1789031488688));
#8295=CARTESIAN_POINT('',(-4.50000000000001,7.,-69.4641016151377));
#8296=CARTESIAN_POINT('',(-4.50000000000001,7.,-69.4641016151377));
#8297=CARTESIAN_POINT('',(-4.50000000000001,7.,-69.4641016151377));
#8298=CARTESIAN_POINT('Origin',(7.5157431494139,7.,-90.2759792406202));
#8299=CARTESIAN_POINT('',(7.5157431494139,7.,-90.2759792406202));
#8300=CARTESIAN_POINT('',(7.5157431494139,7.,-90.2759792406202));
#8301=CARTESIAN_POINT('',(7.5157431494139,7.,-90.2759792406202));
#8302=CARTESIAN_POINT('Origin',(7.5157431494139,7.,-90.2759792406202));
#8303=CARTESIAN_POINT('',(8.5669118613583,7.,-90.4613286458126));
#8304=CARTESIAN_POINT('',(7.5157431494139,7.,-90.2759792406202));
#8305=CARTESIAN_POINT('',(8.5669118613583,7.,-90.4613286458126));
#8306=CARTESIAN_POINT('Origin',(8.5669118613583,7.,-90.4613286458126));
#8307=CARTESIAN_POINT('',(10.5956992404498,7.,-78.9555036669016));
#8308=CARTESIAN_POINT('',(8.5669118613583,7.,-90.4613286458126));
#8309=CARTESIAN_POINT('',(10.5956992404498,7.,-78.9555036669016));
#8310=CARTESIAN_POINT('Origin',(31.3216319671078,7.,-64.9756713141856));
#8311=CARTESIAN_POINT('Origin',(31.3216319671078,7.,-64.9756713141856));
#8312=CARTESIAN_POINT('Origin',(31.3216319671078,7.,-64.9756713141856));
#8313=CARTESIAN_POINT('Origin',(-4.50000000000001,7.,-43.7743150561845));
#8314=CARTESIAN_POINT('',(14.1836440347594,7.,-43.7743150561845));
#8315=CARTESIAN_POINT('',(14.1836440347594,7.,-43.7743150561845));
#8316=CARTESIAN_POINT('',(-4.50000000000001,7.,-43.7743150561845));
#8317=CARTESIAN_POINT('',(-4.50000000000001,7.,-43.7743150561845));
#8318=CARTESIAN_POINT('',(-4.50000000000001,7.,-43.7743150561845));
#8319=CARTESIAN_POINT('Origin',(-4.50000000000001,7.,-67.1547005383792));
#8320=CARTESIAN_POINT('',(-4.50000000000001,7.,-67.1547005383792));
#8321=CARTESIAN_POINT('',(-4.50000000000001,7.,-67.1547005383792));
#8322=CARTESIAN_POINT('',(-4.50000000000001,7.,-67.1547005383792));
#8323=CARTESIAN_POINT('Origin',(-4.50000000000001,7.,-67.1547005383792));
#8324=CARTESIAN_POINT('',(6.6910990889186,7.,-60.6935164668642));
#8325=CARTESIAN_POINT('',(-4.50000000000001,7.,-67.1547005383792));
#8326=CARTESIAN_POINT('',(6.6910990889186,7.,-60.6935164668642));
#8327=CARTESIAN_POINT('Origin',(31.3216319671078,7.,-64.9756713141856));
#8328=CARTESIAN_POINT('',(14.1836440347593,7.,-46.7743150561846));
#8329=CARTESIAN_POINT('Origin',(31.3216319671078,7.,-64.9756713141856));
#8330=CARTESIAN_POINT('',(14.1836440347593,7.,-46.7743150561846));
#8331=CARTESIAN_POINT('Origin',(14.1836440347594,7.,-43.7743150561845));
#8332=CARTESIAN_POINT('',(14.1836440347594,7.,-43.7743150561845));
#8333=CARTESIAN_POINT('Origin',(31.3216319671078,7.,-64.9756713141856));
#8334=CARTESIAN_POINT('Origin',(0.,7.,-7.86046575051991E-16));
#8335=CARTESIAN_POINT('',(3.50000000000001,7.,-2.82842712474618));
#8336=CARTESIAN_POINT('',(3.50000000000001,7.,-2.82842712474618));
#8337=CARTESIAN_POINT('',(-3.50000000000001,7.,-2.82842712474618));
#8338=CARTESIAN_POINT('Origin',(0.,7.,-7.86046575051991E-16));
#8339=CARTESIAN_POINT('',(-3.50000000000001,7.,-2.82842712474618));
#8340=CARTESIAN_POINT('Origin',(-4.50000000000001,7.,-2.82842712474618));
#8341=CARTESIAN_POINT('',(-4.50000000000001,7.,-2.82842712474618));
#8342=CARTESIAN_POINT('',(-4.50000000000001,7.,-2.82842712474618));
#8343=CARTESIAN_POINT('',(-4.50000000000001,7.,-2.82842712474618));
#8344=CARTESIAN_POINT('Origin',(-4.50000000000001,7.,-2.82842712474618));
#8345=CARTESIAN_POINT('',(-4.50000000000001,7.,-41.7743150561845));
#8346=CARTESIAN_POINT('',(-4.50000000000001,7.,-2.82842712474618));
#8347=CARTESIAN_POINT('',(-4.50000000000001,7.,-41.7743150561845));
#8348=CARTESIAN_POINT('Origin',(-4.50000000000001,7.,-41.7743150561845));
#8349=CARTESIAN_POINT('',(14.1836440347594,7.,-41.7743150561845));
#8350=CARTESIAN_POINT('',(-4.50000000000001,7.,-41.7743150561845));
#8351=CARTESIAN_POINT('',(14.1836440347594,7.,-41.7743150561845));
#8352=CARTESIAN_POINT('Origin',(14.1836440347594,7.,-41.7743150561845));
#8353=CARTESIAN_POINT('',(14.1836440347594,7.,-35.7743150561845));
#8354=CARTESIAN_POINT('',(14.1836440347594,7.,-41.7743150561845));
#8355=CARTESIAN_POINT('',(14.1836440347594,7.,-35.7743150561845));
#8356=CARTESIAN_POINT('Origin',(16.5,7.,-24.));
#8357=CARTESIAN_POINT('',(4.50000000000001,7.,-24.));
#8358=CARTESIAN_POINT('Origin',(16.5,7.,-24.));
#8359=CARTESIAN_POINT('',(4.50000000000001,7.,-24.));
#8360=CARTESIAN_POINT('Origin',(4.50000000000001,7.,-2.82842712474618));
#8361=CARTESIAN_POINT('',(4.50000000000001,7.,-2.82842712474618));
#8362=CARTESIAN_POINT('',(4.50000000000001,7.,-2.82842712474618));
#8363=CARTESIAN_POINT('',(4.50000000000001,7.,-2.82842712474618));
#8364=CARTESIAN_POINT('Origin',(3.50000000000001,7.,-2.82842712474618));
#8365=CARTESIAN_POINT('',(3.50000000000001,7.,-2.82842712474618));
#8366=CARTESIAN_POINT('Origin',(0.,7.,-7.86046575051991E-16));
#8367=CARTESIAN_POINT('Origin',(4.50000000000001,1.,-2.82842712474618));
#8368=CARTESIAN_POINT('',(4.50000000000001,1.,-2.82842712474618));
#8369=CARTESIAN_POINT('',(4.50000000000001,1.,-2.82842712474618));
#8370=CARTESIAN_POINT('',(4.50000000000001,1.,-2.82842712474618));
#8371=CARTESIAN_POINT('Origin',(4.50000000000001,1.,-24.));
#8372=CARTESIAN_POINT('',(4.50000000000001,1.,-24.));
#8373=CARTESIAN_POINT('',(4.50000000000001,1.,-24.));
#8374=CARTESIAN_POINT('',(4.50000000000001,1.,-24.));
#8375=CARTESIAN_POINT('Origin',(16.5,1.,-24.));
#8376=CARTESIAN_POINT('',(14.1836440347594,1.,-35.7743150561845));
#8377=CARTESIAN_POINT('Origin',(16.5,1.,-24.));
#8378=CARTESIAN_POINT('',(14.1836440347594,1.,-35.7743150561845));
#8379=CARTESIAN_POINT('Origin',(14.1836440347594,1.,-41.7743150561845));
#8380=CARTESIAN_POINT('',(14.1836440347594,1.,-41.7743150561845));
#8381=CARTESIAN_POINT('',(14.1836440347594,1.,-41.7743150561845));
#8382=CARTESIAN_POINT('',(14.1836440347594,1.,-41.7743150561845));
#8383=CARTESIAN_POINT('Origin',(-4.50000000000001,1.,-41.7743150561845));
#8384=CARTESIAN_POINT('',(-4.50000000000001,1.,-41.7743150561845));
#8385=CARTESIAN_POINT('',(-4.50000000000001,1.,-41.7743150561845));
#8386=CARTESIAN_POINT('',(-4.50000000000001,1.,-41.7743150561845));
#8387=CARTESIAN_POINT('Origin',(-4.50000000000001,1.,-2.82842712474618));
#8388=CARTESIAN_POINT('',(-4.50000000000001,1.,-2.82842712474618));
#8389=CARTESIAN_POINT('',(-4.50000000000001,1.,-2.82842712474618));
#8390=CARTESIAN_POINT('',(-4.50000000000001,1.,-2.82842712474618));
#8391=CARTESIAN_POINT('Origin',(-3.50000000000001,1.,-2.82842712474618));
#8392=CARTESIAN_POINT('',(-3.50000000000001,1.,-2.82842712474618));
#8393=CARTESIAN_POINT('Origin',(0.,1.,-7.86046575051991E-16));
#8394=CARTESIAN_POINT('Origin',(-4.50000000000001,1.,-69.4641016151377));
#8395=CARTESIAN_POINT('',(7.5157431494139,1.,-90.2759792406202));
#8396=CARTESIAN_POINT('',(7.5157431494139,1.,-90.2759792406202));
#8397=CARTESIAN_POINT('',(-4.50000000000001,1.,-69.4641016151377));
#8398=CARTESIAN_POINT('',(-4.50000000000001,1.,-69.4641016151377));
#8399=CARTESIAN_POINT('',(-4.50000000000001,1.,-69.4641016151377));
#8400=CARTESIAN_POINT('Origin',(6.38628307923175,1.,-63.1789031488688));
#8401=CARTESIAN_POINT('',(6.38628307923175,1.,-63.1789031488688));
#8402=CARTESIAN_POINT('',(6.38628307923175,1.,-63.1789031488688));
#8403=CARTESIAN_POINT('',(6.38628307923175,1.,-63.1789031488688));
#8404=CARTESIAN_POINT('Origin',(31.3216319671078,1.,-64.9756713141856));
#8405=CARTESIAN_POINT('',(10.5956992404498,1.,-78.9555036669016));
#8406=CARTESIAN_POINT('Origin',(31.3216319671078,1.,-64.9756713141856));
#8407=CARTESIAN_POINT('',(10.5956992404498,1.,-78.9555036669016));
#8408=CARTESIAN_POINT('Origin',(8.5669118613583,1.,-90.4613286458126));
#8409=CARTESIAN_POINT('',(8.5669118613583,1.,-90.4613286458126));
#8410=CARTESIAN_POINT('',(8.5669118613583,1.,-90.4613286458126));
#8411=CARTESIAN_POINT('',(8.5669118613583,1.,-90.4613286458126));
#8412=CARTESIAN_POINT('Origin',(7.5157431494139,1.,-90.2759792406202));
#8413=CARTESIAN_POINT('',(7.5157431494139,1.,-90.2759792406202));
#8414=CARTESIAN_POINT('Origin',(31.3216319671078,1.,-64.9756713141856));
#8415=CARTESIAN_POINT('Origin',(-4.50000000000001,1.,-43.7743150561845));
#8416=CARTESIAN_POINT('',(-4.50000000000001,1.,-67.1547005383792));
#8417=CARTESIAN_POINT('',(-4.50000000000001,1.,-67.1547005383792));
#8418=CARTESIAN_POINT('',(-4.50000000000001,1.,-43.7743150561845));
#8419=CARTESIAN_POINT('',(-4.50000000000001,1.,-43.7743150561845));
#8420=CARTESIAN_POINT('',(-4.50000000000001,1.,-43.7743150561845));
#8421=CARTESIAN_POINT('Origin',(14.1836440347594,1.,-43.7743150561845));
#8422=CARTESIAN_POINT('',(14.1836440347594,1.,-43.7743150561845));
#8423=CARTESIAN_POINT('',(14.1836440347594,1.,-43.7743150561845));
#8424=CARTESIAN_POINT('',(14.1836440347594,1.,-43.7743150561845));
#8425=CARTESIAN_POINT('Origin',(14.1836440347593,1.,-46.7743150561846));
#8426=CARTESIAN_POINT('',(14.1836440347593,1.,-46.7743150561846));
#8427=CARTESIAN_POINT('',(14.1836440347593,1.,-46.7743150561846));
#8428=CARTESIAN_POINT('',(14.1836440347593,1.,-46.7743150561846));
#8429=CARTESIAN_POINT('Origin',(31.3216319671078,1.,-64.9756713141856));
#8430=CARTESIAN_POINT('',(6.6910990889186,1.,-60.6935164668642));
#8431=CARTESIAN_POINT('Origin',(31.3216319671078,1.,-64.9756713141856));
#8432=CARTESIAN_POINT('',(6.6910990889186,1.,-60.6935164668642));
#8433=CARTESIAN_POINT('Origin',(-4.50000000000001,1.,-67.1547005383792));
#8434=CARTESIAN_POINT('',(-4.50000000000001,1.,-67.1547005383792));
#8435=CARTESIAN_POINT('Origin',(31.3216319671078,1.,-64.9756713141856));
#8436=CARTESIAN_POINT('',(0.,0.,0.));
#8437=CARTESIAN_POINT('Origin',(0.,0.,1.));
#8438=CARTESIAN_POINT('',(7.,-8.57252759403147E-16,0.));
#8439=CARTESIAN_POINT('Origin',(0.,0.,0.));
#8440=CARTESIAN_POINT('',(7.,-8.57252759403147E-16,1.));
#8441=CARTESIAN_POINT('',(7.,-8.57252759403147E-16,1.));
#8442=CARTESIAN_POINT('Origin',(0.,0.,1.));
#8443=CARTESIAN_POINT('Origin',(0.,0.,1.));
#8444=CARTESIAN_POINT('',(14.,-1.71450551880629E-15,1.));
#8445=CARTESIAN_POINT('Origin',(0.,0.,1.));
#8446=CARTESIAN_POINT('',(14.,-1.71450551880629E-15,0.));
#8447=CARTESIAN_POINT('',(14.,-1.71450551880629E-15,1.));
#8448=CARTESIAN_POINT('Origin',(0.,0.,0.));
#8449=CARTESIAN_POINT('Origin',(0.,0.,6.));
#8450=CARTESIAN_POINT('',(-7.,-8.57252759403147E-16,7.));
#8451=CARTESIAN_POINT('Origin',(0.,0.,7.));
#8452=CARTESIAN_POINT('',(-7.,-8.57252759403147E-16,6.));
#8453=CARTESIAN_POINT('',(-7.,-8.57252759403147E-16,6.));
#8454=CARTESIAN_POINT('Origin',(0.,0.,6.));
#8455=CARTESIAN_POINT('Origin',(0.,0.,6.));
#8456=CARTESIAN_POINT('',(-14.,-1.71450551880629E-15,6.));
#8457=CARTESIAN_POINT('Origin',(0.,0.,6.));
#8458=CARTESIAN_POINT('',(-14.,-1.71450551880629E-15,7.));
#8459=CARTESIAN_POINT('',(-14.,-1.71450551880629E-15,6.));
#8460=CARTESIAN_POINT('Origin',(0.,0.,7.));
#8461=CARTESIAN_POINT('Origin',(0.,-2.16840434497101E-15,7.));
#8462=CARTESIAN_POINT('',(2.5,-2.47456604475785E-15,7.));
#8463=CARTESIAN_POINT('Origin',(0.,-2.16840434497101E-15,7.));
#8464=CARTESIAN_POINT('',(2.5,-2.47456604475785E-15,0.));
#8465=CARTESIAN_POINT('',(2.5,-2.47456604475785E-15,7.));
#8466=CARTESIAN_POINT('Origin',(0.,-2.16840434497101E-15,0.));
#8467=CARTESIAN_POINT('Origin',(0.,0.,7.));
#8468=CARTESIAN_POINT('',(-16.2160625265911,1.04967429885986,7.));
#8469=CARTESIAN_POINT('',(-16.2160625265912,-1.04967429885971,7.));
#8470=CARTESIAN_POINT('Origin',(0.,0.,7.));
#8471=CARTESIAN_POINT('',(-16.2160625265911,1.04967429885986,0.));
#8472=CARTESIAN_POINT('',(-16.2160625265911,1.04967429885986,7.));
#8473=CARTESIAN_POINT('',(-16.2160625265912,-1.04967429885971,0.));
#8474=CARTESIAN_POINT('Origin',(0.,0.,0.));
#8475=CARTESIAN_POINT('',(-16.2160625265912,-1.04967429885971,7.));
#8476=CARTESIAN_POINT('Origin',(16.0675296603332,7.07348467874013,0.));
#8477=CARTESIAN_POINT('Origin',(16.0675296603332,7.07348467874013,7.));
#8478=CARTESIAN_POINT('Origin',(16.0675296603332,7.07348467874013,7.));
#8479=CARTESIAN_POINT('',(15.0980247376579,6.00933848448158,7.));
#8480=CARTESIAN_POINT('',(17.1502563092004,8.17732893607278,7.));
#8481=CARTESIAN_POINT('Ctrl Pts',(15.0980247376579,6.00933848448158,7.));
#8482=CARTESIAN_POINT('Ctrl Pts',(15.0769402326058,6.07637133495396,7.));
#8483=CARTESIAN_POINT('Ctrl Pts',(15.0680440207731,6.1960413432609,7.));
#8484=CARTESIAN_POINT('Ctrl Pts',(15.1168047097502,6.34385243988821,7.));
#8485=CARTESIAN_POINT('Ctrl Pts',(15.1795880240196,6.44397890908497,7.));
#8486=CARTESIAN_POINT('Ctrl Pts',(15.2506809503975,6.52246995302229,7.));
#8487=CARTESIAN_POINT('Ctrl Pts',(15.3282076647862,6.58832104206024,7.));
#8488=CARTESIAN_POINT('Ctrl Pts',(15.3933171197393,6.63306845520277,7.));
#8489=CARTESIAN_POINT('Ctrl Pts',(15.4424051151807,6.66297054550544,7.));
#8490=CARTESIAN_POINT('Ctrl Pts',(15.4733031879166,6.68074830397728,7.));
#8491=CARTESIAN_POINT('Ctrl Pts',(15.5083268912119,6.69953551835471,7.));
#8492=CARTESIAN_POINT('Ctrl Pts',(15.5619248294191,6.72790031412625,7.));
#8493=CARTESIAN_POINT('Ctrl Pts',(15.6387111659832,6.77211692048664,7.));
#8494=CARTESIAN_POINT('Ctrl Pts',(15.7406883947778,6.83570676658069,7.));
#8495=CARTESIAN_POINT('Ctrl Pts',(15.8583036897433,6.91534043556371,7.));
#8496=CARTESIAN_POINT('Ctrl Pts',(15.9905219781863,7.01217619187965,7.));
#8497=CARTESIAN_POINT('Ctrl Pts',(16.1361838672874,7.12742326811382,7.));
#8498=CARTESIAN_POINT('Ctrl Pts',(16.2940809887434,7.2621916599568,7.));
#8499=CARTESIAN_POINT('Ctrl Pts',(16.4629349257385,7.41753779118422,7.));
#8500=CARTESIAN_POINT('Ctrl Pts',(16.6414085620714,7.59444470905136,7.));
#8501=CARTESIAN_POINT('Ctrl Pts',(16.8766905033057,7.84571320523309,7.));
#8502=CARTESIAN_POINT('Ctrl Pts',(17.0448123137865,8.04476736935674,7.));
#8503=CARTESIAN_POINT('Ctrl Pts',(17.1502563092004,8.17732893607278,7.));
#8504=CARTESIAN_POINT('',(16.6962658094608,9.06833546026115,7.));
#8505=CARTESIAN_POINT('Origin',(2.16840434497101E-15,0.,7.));
#8506=CARTESIAN_POINT('',(13.7360532384392,8.6823580570467,7.));
#8507=CARTESIAN_POINT('Ctrl Pts',(16.6962658094608,9.06833546026115,7.));
#8508=CARTESIAN_POINT('Ctrl Pts',(16.5270428237395,9.06094720995301,7.));
#8509=CARTESIAN_POINT('Ctrl Pts',(16.267185101373,9.0419349102283,7.));
#8510=CARTESIAN_POINT('Ctrl Pts',(15.9256093626227,8.9992797377215,7.));
#8511=CARTESIAN_POINT('Ctrl Pts',(15.6775844882862,8.95887481023115,7.));
#8512=CARTESIAN_POINT('Ctrl Pts',(15.4526569741556,8.9135792705712,7.));
#8513=CARTESIAN_POINT('Ctrl Pts',(15.2508174554787,8.86505268915081,7.));
#8514=CARTESIAN_POINT('Ctrl Pts',(15.0719627020186,8.8149502772156,7.));
#8515=CARTESIAN_POINT('Ctrl Pts',(14.9159049694657,8.76490206435509,7.));
#8516=CARTESIAN_POINT('Ctrl Pts',(14.7823474421092,8.71655678814372,7.));
#8517=CARTESIAN_POINT('Ctrl Pts',(14.6709614647943,8.67143265073928,7.));
#8518=CARTESIAN_POINT('Ctrl Pts',(14.5900556026053,8.63530106864818,7.));
#8519=CARTESIAN_POINT('Ctrl Pts',(14.5356039231526,8.60861183441388,7.));
#8520=CARTESIAN_POINT('Ctrl Pts',(14.4998183311667,8.59131991078479,7.));
#8521=CARTESIAN_POINT('Ctrl Pts',(14.4672743909626,8.57677234909658,7.));
#8522=CARTESIAN_POINT('Ctrl Pts',(14.4142298919554,8.55463533425733,7.));
#8523=CARTESIAN_POINT('Ctrl Pts',(14.3397580968625,8.52826254822916,7.));
#8524=CARTESIAN_POINT('Ctrl Pts',(14.2409143873564,8.50424841775457,7.));
#8525=CARTESIAN_POINT('Ctrl Pts',(14.1356264252376,8.49286891019843,7.));
#8526=CARTESIAN_POINT('Ctrl Pts',(14.0177193038531,8.5009290039492,7.));
#8527=CARTESIAN_POINT('Ctrl Pts',(13.8694768008521,8.54836196063209,7.));
#8528=CARTESIAN_POINT('Ctrl Pts',(13.7778907925312,8.62589941321481,7.));
#8529=CARTESIAN_POINT('Ctrl Pts',(13.7360532384392,8.6823580570467,7.));
#8530=CARTESIAN_POINT('',(12.5020870932787,10.3807667497191,7.));
#8531=CARTESIAN_POINT('Origin',(0.,0.,7.));
#8532=CARTESIAN_POINT('',(13.7839294091566,13.07682262797,7.));
#8533=CARTESIAN_POINT('Ctrl Pts',(12.5020870932787,10.3807667497191,7.));
#8534=CARTESIAN_POINT('Ctrl Pts',(12.4613202473788,10.4380033085876,7.));
#8535=CARTESIAN_POINT('Ctrl Pts',(12.4158793808611,10.5490671691512,7.));
#8536=CARTESIAN_POINT('Ctrl Pts',(12.4165774110367,10.7047117573306,7.));
#8537=CARTESIAN_POINT('Ctrl Pts',(12.4453471106188,10.8193387993863,7.));
#8538=CARTESIAN_POINT('Ctrl Pts',(12.48870543503,10.9159571406243,7.));
#8539=CARTESIAN_POINT('Ctrl Pts',(12.5420886163255,11.0025423202231,7.));
#8540=CARTESIAN_POINT('Ctrl Pts',(12.5901836766158,11.0652195671547,7.));
#8541=CARTESIAN_POINT('Ctrl Pts',(12.6276288804813,11.1088271697991,7.));
#8542=CARTESIAN_POINT('Ctrl Pts',(12.651521064408,11.1352828524077,7.));
#8543=CARTESIAN_POINT('Ctrl Pts',(12.6790250171322,11.1639734745885,7.));
#8544=CARTESIAN_POINT('Ctrl Pts',(12.7212344815888,11.2075126722099,7.));
#8545=CARTESIAN_POINT('Ctrl Pts',(12.7805989445416,11.2732934467515,7.));
#8546=CARTESIAN_POINT('Ctrl Pts',(12.8579347093876,11.3652836809863,7.));
#8547=CARTESIAN_POINT('Ctrl Pts',(12.9451853450404,11.4773649257318,7.));
#8548=CARTESIAN_POINT('Ctrl Pts',(13.0410085154727,11.6103189008825,7.));
#8549=CARTESIAN_POINT('Ctrl Pts',(13.1439278991698,11.764937382884,7.));
#8550=CARTESIAN_POINT('Ctrl Pts',(13.2524512620507,11.9419026340297,7.));
#8551=CARTESIAN_POINT('Ctrl Pts',(13.3650363045724,12.1418243205134,7.));
#8552=CARTESIAN_POINT('Ctrl Pts',(13.4801075753502,12.3652241842034,7.));
#8553=CARTESIAN_POINT('Ctrl Pts',(13.6262277632565,12.6769008431476,7.));
#8554=CARTESIAN_POINT('Ctrl Pts',(13.7246099871303,12.9181650995967,7.));
#8555=CARTESIAN_POINT('Ctrl Pts',(13.7839294091566,13.07682262797,7.));
#8556=CARTESIAN_POINT('',(13.07682262797,13.7839294091566,7.));
#8557=CARTESIAN_POINT('Origin',(0.,0.,7.));
#8558=CARTESIAN_POINT('',(10.3807667497191,12.5020870932787,7.));
#8559=CARTESIAN_POINT('Ctrl Pts',(13.07682262797,13.7839294091566,7.));
#8560=CARTESIAN_POINT('Ctrl Pts',(12.9181650995967,13.7246099871302,7.));
#8561=CARTESIAN_POINT('Ctrl Pts',(12.6769008431476,13.6262277632565,7.));
#8562=CARTESIAN_POINT('Ctrl Pts',(12.3652241842033,13.4801075753502,7.));
#8563=CARTESIAN_POINT('Ctrl Pts',(12.1418243205134,13.3650363045723,7.));
#8564=CARTESIAN_POINT('Ctrl Pts',(11.9419026340297,13.2524512620508,7.));
#8565=CARTESIAN_POINT('Ctrl Pts',(11.764937382884,13.1439278991698,7.));
#8566=CARTESIAN_POINT('Ctrl Pts',(11.6103189008825,13.0410085154728,7.));
#8567=CARTESIAN_POINT('Ctrl Pts',(11.4773649257318,12.9451853450404,7.));
#8568=CARTESIAN_POINT('Ctrl Pts',(11.3652836809863,12.8579347093876,7.));
#8569=CARTESIAN_POINT('Ctrl Pts',(11.2732934467515,12.7805989445416,7.));
#8570=CARTESIAN_POINT('Ctrl Pts',(11.2075126722099,12.7212344815888,7.));
#8571=CARTESIAN_POINT('Ctrl Pts',(11.1639734745885,12.6790250171322,7.));
#8572=CARTESIAN_POINT('Ctrl Pts',(11.1352828524076,12.6515210644081,7.));
#8573=CARTESIAN_POINT('Ctrl Pts',(11.108827169799,12.6276288804813,7.));
#8574=CARTESIAN_POINT('Ctrl Pts',(11.0652195671547,12.5901836766158,7.));
#8575=CARTESIAN_POINT('Ctrl Pts',(11.0025423202231,12.5420886163255,7.));
#8576=CARTESIAN_POINT('Ctrl Pts',(10.9159571406242,12.48870543503,7.));
#8577=CARTESIAN_POINT('Ctrl Pts',(10.8193387993863,12.4453471106187,7.));
#8578=CARTESIAN_POINT('Ctrl Pts',(10.7047117573306,12.4165774110367,7.));
#8579=CARTESIAN_POINT('Ctrl Pts',(10.5490671691512,12.4158793808611,7.));
#8580=CARTESIAN_POINT('Ctrl Pts',(10.4380033085876,12.4613202473787,7.));
#8581=CARTESIAN_POINT('Ctrl Pts',(10.3807667497191,12.5020870932787,7.));
#8582=CARTESIAN_POINT('',(8.68235805704686,13.7360532384391,7.));
#8583=CARTESIAN_POINT('Origin',(0.,0.,7.));
#8584=CARTESIAN_POINT('',(9.06833546026116,16.6962658094608,7.));
#8585=CARTESIAN_POINT('Ctrl Pts',(8.68235805704686,13.7360532384391,7.));
#8586=CARTESIAN_POINT('Ctrl Pts',(8.62589941321482,13.7778907925313,7.));
#8587=CARTESIAN_POINT('Ctrl Pts',(8.54836196063209,13.8694768008521,7.));
#8588=CARTESIAN_POINT('Ctrl Pts',(8.50092900394922,14.0177193038531,7.));
#8589=CARTESIAN_POINT('Ctrl Pts',(8.49286891019844,14.1356264252377,7.));
#8590=CARTESIAN_POINT('Ctrl Pts',(8.50424841775457,14.2409143873564,7.));
#8591=CARTESIAN_POINT('Ctrl Pts',(8.52826254822916,14.3397580968626,7.));
#8592=CARTESIAN_POINT('Ctrl Pts',(8.55463533425733,14.4142298919554,7.));
#8593=CARTESIAN_POINT('Ctrl Pts',(8.57677234909656,14.4672743909627,7.));
#8594=CARTESIAN_POINT('Ctrl Pts',(8.59131991078476,14.4998183311667,7.));
#8595=CARTESIAN_POINT('Ctrl Pts',(8.6086118344139,14.5356039231527,7.));
#8596=CARTESIAN_POINT('Ctrl Pts',(8.63530106864819,14.5900556026053,7.));
#8597=CARTESIAN_POINT('Ctrl Pts',(8.67143265073928,14.6709614647944,7.));
#8598=CARTESIAN_POINT('Ctrl Pts',(8.71655678814373,14.7823474421093,7.));
#8599=CARTESIAN_POINT('Ctrl Pts',(8.76490206435509,14.9159049694657,7.));
#8600=CARTESIAN_POINT('Ctrl Pts',(8.81495027721557,15.0719627020186,7.));
#8601=CARTESIAN_POINT('Ctrl Pts',(8.86505268915084,15.2508174554788,7.));
#8602=CARTESIAN_POINT('Ctrl Pts',(8.91357927057117,15.4526569741556,7.));
#8603=CARTESIAN_POINT('Ctrl Pts',(8.95887481023115,15.6775844882862,7.));
#8604=CARTESIAN_POINT('Ctrl Pts',(8.99927973772153,15.9256093626227,7.));
#8605=CARTESIAN_POINT('Ctrl Pts',(9.04193491022831,16.2671851013731,7.));
#8606=CARTESIAN_POINT('Ctrl Pts',(9.06094720995305,16.5270428237395,7.));
#8607=CARTESIAN_POINT('Ctrl Pts',(9.06833546026116,16.6962658094608,7.));
#8608=CARTESIAN_POINT('',(8.17732893607301,17.1502563092002,7.));
#8609=CARTESIAN_POINT('Origin',(0.,-2.16840434497101E-15,7.));
#8610=CARTESIAN_POINT('',(6.00933848448158,15.0980247376579,7.));
#8611=CARTESIAN_POINT('Ctrl Pts',(8.17732893607301,17.1502563092002,7.));
#8612=CARTESIAN_POINT('Ctrl Pts',(8.04476736935673,17.0448123137865,7.));
#8613=CARTESIAN_POINT('Ctrl Pts',(7.84571320523309,16.8766905033057,7.));
#8614=CARTESIAN_POINT('Ctrl Pts',(7.59444470905135,16.6414085620714,7.));
#8615=CARTESIAN_POINT('Ctrl Pts',(7.4175377911842,16.4629349257385,7.));
#8616=CARTESIAN_POINT('Ctrl Pts',(7.26219165995678,16.2940809887434,7.));
#8617=CARTESIAN_POINT('Ctrl Pts',(7.12742326811382,16.1361838672874,7.));
#8618=CARTESIAN_POINT('Ctrl Pts',(7.01217619187961,15.9905219781863,7.));
#8619=CARTESIAN_POINT('Ctrl Pts',(6.91534043556368,15.8583036897433,7.));
#8620=CARTESIAN_POINT('Ctrl Pts',(6.83570676658068,15.7406883947777,7.));
#8621=CARTESIAN_POINT('Ctrl Pts',(6.77211692048662,15.6387111659832,7.));
#8622=CARTESIAN_POINT('Ctrl Pts',(6.72790031412623,15.5619248294191,7.));
#8623=CARTESIAN_POINT('Ctrl Pts',(6.69953551835472,15.5083268912119,7.));
#8624=CARTESIAN_POINT('Ctrl Pts',(6.68074830397725,15.4733031879166,7.));
#8625=CARTESIAN_POINT('Ctrl Pts',(6.66297054550541,15.4424051151807,7.));
#8626=CARTESIAN_POINT('Ctrl Pts',(6.63306845520275,15.3933171197393,7.));
#8627=CARTESIAN_POINT('Ctrl Pts',(6.58832104206022,15.3282076647862,7.));
#8628=CARTESIAN_POINT('Ctrl Pts',(6.52246995302225,15.2506809503975,7.));
#8629=CARTESIAN_POINT('Ctrl Pts',(6.44397890908495,15.1795880240196,7.));
#8630=CARTESIAN_POINT('Ctrl Pts',(6.34385243988822,15.1168047097501,7.));
#8631=CARTESIAN_POINT('Ctrl Pts',(6.19604134326089,15.0680440207731,7.));
#8632=CARTESIAN_POINT('Ctrl Pts',(6.07637133495393,15.0769402326058,7.));
#8633=CARTESIAN_POINT('Ctrl Pts',(6.00933848448158,15.0980247376579,7.));
#8634=CARTESIAN_POINT('',(4.01273932064543,15.7467591314704,7.));
#8635=CARTESIAN_POINT('Origin',(0.,0.,7.));
#8636=CARTESIAN_POINT('',(3.46506965370702,18.6813621637974,7.));
#8637=CARTESIAN_POINT('Ctrl Pts',(4.01273932064543,15.7467591314704,7.));
#8638=CARTESIAN_POINT('Ctrl Pts',(3.94611544431017,15.7691023294921,7.));
#8639=CARTESIAN_POINT('Ctrl Pts',(3.84407131175635,15.8322454089585,7.));
#8640=CARTESIAN_POINT('Ctrl Pts',(3.75315043649997,15.9585748177211,7.));
#8641=CARTESIAN_POINT('Ctrl Pts',(3.70904952755068,16.0682204478862,7.));
#8642=CARTESIAN_POINT('Ctrl Pts',(3.68733631276637,16.1718717115691,7.));
#8643=CARTESIAN_POINT('Ctrl Pts',(3.67963072201293,16.2732984400116,7.));
#8644=CARTESIAN_POINT('Ctrl Pts',(3.68169968173257,16.3522749650866,7.));
#8645=CARTESIAN_POINT('Ctrl Pts',(3.68636158229542,16.409563995311,7.));
#8646=CARTESIAN_POINT('Ctrl Pts',(3.69014050504822,16.4450105654964,7.));
#8647=CARTESIAN_POINT('Ctrl Pts',(3.69552774561756,16.4843881842109,7.));
#8648=CARTESIAN_POINT('Ctrl Pts',(3.70408422142788,16.5444222357228,7.));
#8649=CARTESIAN_POINT('Ctrl Pts',(3.71344611165869,16.632533556064,7.));
#8650=CARTESIAN_POINT('Ctrl Pts',(3.72194155665403,16.7524120409277,7.));
#8651=CARTESIAN_POINT('Ctrl Pts',(3.7266491009471,16.8943723095674,7.));
#8652=CARTESIAN_POINT('Ctrl Pts',(3.72602328845452,17.0582577813421,7.));
#8653=CARTESIAN_POINT('Ctrl Pts',(3.71840435546373,17.2438412568379,7.));
#8654=CARTESIAN_POINT('Ctrl Pts',(3.70218403552947,17.4507975846592,7.));
#8655=CARTESIAN_POINT('Ctrl Pts',(3.67575622931333,17.6787134541915,7.));
#8656=CARTESIAN_POINT('Ctrl Pts',(3.63753969769581,17.9270849363835,7.));
#8657=CARTESIAN_POINT('Ctrl Pts',(3.57255446932205,18.265123941733,7.));
#8658=CARTESIAN_POINT('Ctrl Pts',(3.51033578853423,18.5181384456163,7.));
#8659=CARTESIAN_POINT('Ctrl Pts',(3.46506965370702,18.6813621637974,7.));
#8660=CARTESIAN_POINT('',(2.47738131311212,18.8377966288375,7.));
#8661=CARTESIAN_POINT('Origin',(0.,8.67361737988404E-16,7.));
#8662=CARTESIAN_POINT('',(1.04967429885989,16.2160625265911,7.));
#8663=CARTESIAN_POINT('Ctrl Pts',(2.47738131311212,18.8377966288375,7.));
#8664=CARTESIAN_POINT('Ctrl Pts',(2.38389175781397,18.6965496529788,7.));
#8665=CARTESIAN_POINT('Ctrl Pts',(2.24653249449213,18.4751451900744,7.));
#8666=CARTESIAN_POINT('Ctrl Pts',(2.08026807216976,18.1737325312257,7.));
#8667=CARTESIAN_POINT('Ctrl Pts',(1.96717098182927,17.949326772361,7.));
#8668=CARTESIAN_POINT('Ctrl Pts',(1.87160676754279,17.7407325407201,7.));
#8669=CARTESIAN_POINT('Ctrl Pts',(1.79222730418274,17.548917731071,7.));
#8670=CARTESIAN_POINT('Ctrl Pts',(1.72763282051121,17.3747717371572,7.));
#8671=CARTESIAN_POINT('Ctrl Pts',(1.67639424155266,17.2191007779952,7.));
#8672=CARTESIAN_POINT('Ctrl Pts',(1.63700324669265,17.0826338282621,7.));
#8673=CARTESIAN_POINT('Ctrl Pts',(1.60803840593148,16.9659973771906,7.));
#8674=CARTESIAN_POINT('Ctrl Pts',(1.58971419725808,16.8793055486399,7.));
#8675=CARTESIAN_POINT('Ctrl Pts',(1.57930034717568,16.8195656763126,7.));
#8676=CARTESIAN_POINT('Ctrl Pts',(1.57225556404314,16.7804505865492,7.));
#8677=CARTESIAN_POINT('Ctrl Pts',(1.5648959405722,16.7455711436431,7.));
#8678=CARTESIAN_POINT('Ctrl Pts',(1.5516263875502,16.6896454316358,7.));
#8679=CARTESIAN_POINT('Ctrl Pts',(1.52918899676866,16.6138949491149,7.));
#8680=CARTESIAN_POINT('Ctrl Pts',(1.49051796169813,16.5198135565977,7.));
#8681=CARTESIAN_POINT('Ctrl Pts',(1.43783746532136,16.4279450992207,7.));
#8682=CARTESIAN_POINT('Ctrl Pts',(1.36201264541063,16.3372938385016,7.));
#8683=CARTESIAN_POINT('Ctrl Pts',(1.23650382033381,16.2452435266959,7.));
#8684=CARTESIAN_POINT('Ctrl Pts',(1.11994179848653,16.2167242606458,7.));
#8685=CARTESIAN_POINT('Ctrl Pts',(1.04967429885989,16.2160625265911,7.));
#8686=CARTESIAN_POINT('',(-1.04967429885962,16.2160625265911,7.));
#8687=CARTESIAN_POINT('Origin',(0.,0.,7.));
#8688=CARTESIAN_POINT('',(-2.47738131311187,18.8377966288376,7.));
#8689=CARTESIAN_POINT('Ctrl Pts',(-1.04967429885962,16.2160625265911,7.));
#8690=CARTESIAN_POINT('Ctrl Pts',(-1.11994179848651,16.2167242606459,7.));
#8691=CARTESIAN_POINT('Ctrl Pts',(-1.23650382033378,16.2452435266959,7.));
#8692=CARTESIAN_POINT('Ctrl Pts',(-1.36201264541058,16.3372938385016,7.));
#8693=CARTESIAN_POINT('Ctrl Pts',(-1.43783746532133,16.4279450992208,7.));
#8694=CARTESIAN_POINT('Ctrl Pts',(-1.49051796169812,16.5198135565978,7.));
#8695=CARTESIAN_POINT('Ctrl Pts',(-1.52918899676864,16.6138949491149,7.));
#8696=CARTESIAN_POINT('Ctrl Pts',(-1.55162638755018,16.6896454316359,7.));
#8697=CARTESIAN_POINT('Ctrl Pts',(-1.5648959405722,16.7455711436431,7.));
#8698=CARTESIAN_POINT('Ctrl Pts',(-1.57225556404314,16.7804505865492,7.));
#8699=CARTESIAN_POINT('Ctrl Pts',(-1.57930034717564,16.8195656763126,7.));
#8700=CARTESIAN_POINT('Ctrl Pts',(-1.58971419725806,16.8793055486399,7.));
#8701=CARTESIAN_POINT('Ctrl Pts',(-1.60803840593146,16.9659973771906,7.));
#8702=CARTESIAN_POINT('Ctrl Pts',(-1.63700324669262,17.0826338282622,7.));
#8703=CARTESIAN_POINT('Ctrl Pts',(-1.67639424155265,17.2191007779953,7.));
#8704=CARTESIAN_POINT('Ctrl Pts',(-1.72763282051122,17.3747717371572,7.));
#8705=CARTESIAN_POINT('Ctrl Pts',(-1.7922273041827,17.548917731071,7.));
#8706=CARTESIAN_POINT('Ctrl Pts',(-1.87160676754278,17.7407325407201,7.));
#8707=CARTESIAN_POINT('Ctrl Pts',(-1.96717098182926,17.949326772361,7.));
#8708=CARTESIAN_POINT('Ctrl Pts',(-2.08026807216973,18.1737325312257,7.));
#8709=CARTESIAN_POINT('Ctrl Pts',(-2.24653249449211,18.4751451900744,7.));
#8710=CARTESIAN_POINT('Ctrl Pts',(-2.38389175781394,18.6965496529788,7.));
#8711=CARTESIAN_POINT('Ctrl Pts',(-2.47738131311187,18.8377966288376,7.));
#8712=CARTESIAN_POINT('',(-3.46506965370679,18.6813621637974,7.));
#8713=CARTESIAN_POINT('Origin',(-1.73472347597681E-15,0.,7.));
#8714=CARTESIAN_POINT('',(-4.01273932064518,15.7467591314705,7.));
#8715=CARTESIAN_POINT('Ctrl Pts',(-3.46506965370679,18.6813621637974,7.));
#8716=CARTESIAN_POINT('Ctrl Pts',(-3.51033578853418,18.5181384456162,7.));
#8717=CARTESIAN_POINT('Ctrl Pts',(-3.57255446932203,18.265123941733,7.));
#8718=CARTESIAN_POINT('Ctrl Pts',(-3.63753969769577,17.9270849363835,7.));
#8719=CARTESIAN_POINT('Ctrl Pts',(-3.67575622931332,17.6787134541915,7.));
#8720=CARTESIAN_POINT('Ctrl Pts',(-3.70218403552948,17.4507975846592,7.));
#8721=CARTESIAN_POINT('Ctrl Pts',(-3.7184043554637,17.2438412568379,7.));
#8722=CARTESIAN_POINT('Ctrl Pts',(-3.72602328845454,17.0582577813421,7.));
#8723=CARTESIAN_POINT('Ctrl Pts',(-3.72664910094709,16.8943723095674,7.));
#8724=CARTESIAN_POINT('Ctrl Pts',(-3.72194155665401,16.7524120409277,7.));
#8725=CARTESIAN_POINT('Ctrl Pts',(-3.71344611165868,16.632533556064,7.));
#8726=CARTESIAN_POINT('Ctrl Pts',(-3.70408422142788,16.5444222357228,7.));
#8727=CARTESIAN_POINT('Ctrl Pts',(-3.69552774561753,16.4843881842109,7.));
#8728=CARTESIAN_POINT('Ctrl Pts',(-3.69014050504823,16.4450105654964,7.));
#8729=CARTESIAN_POINT('Ctrl Pts',(-3.68636158229542,16.409563995311,7.));
#8730=CARTESIAN_POINT('Ctrl Pts',(-3.68169968173256,16.3522749650865,7.));
#8731=CARTESIAN_POINT('Ctrl Pts',(-3.67963072201293,16.2732984400115,7.));
#8732=CARTESIAN_POINT('Ctrl Pts',(-3.68733631276638,16.1718717115691,7.));
#8733=CARTESIAN_POINT('Ctrl Pts',(-3.70904952755066,16.0682204478862,7.));
#8734=CARTESIAN_POINT('Ctrl Pts',(-3.75315043649994,15.958574817721,7.));
#8735=CARTESIAN_POINT('Ctrl Pts',(-3.84407131175633,15.8322454089585,7.));
#8736=CARTESIAN_POINT('Ctrl Pts',(-3.94611544431016,15.7691023294921,7.));
#8737=CARTESIAN_POINT('Ctrl Pts',(-4.01273932064518,15.7467591314705,7.));
#8738=CARTESIAN_POINT('',(-6.00933848448141,15.0980247376579,7.));
#8739=CARTESIAN_POINT('Origin',(0.,0.,7.));
#8740=CARTESIAN_POINT('',(-8.1773289360728,17.1502563092004,7.));
#8741=CARTESIAN_POINT('Ctrl Pts',(-6.00933848448141,15.0980247376579,7.));
#8742=CARTESIAN_POINT('Ctrl Pts',(-6.076371334954,15.0769402326058,7.));
#8743=CARTESIAN_POINT('Ctrl Pts',(-6.19604134326094,15.0680440207731,7.));
#8744=CARTESIAN_POINT('Ctrl Pts',(-6.34385243988825,15.1168047097501,7.));
#8745=CARTESIAN_POINT('Ctrl Pts',(-6.44397890908501,15.1795880240196,7.));
#8746=CARTESIAN_POINT('Ctrl Pts',(-6.52246995302233,15.2506809503975,7.));
#8747=CARTESIAN_POINT('Ctrl Pts',(-6.58832104206028,15.3282076647862,7.));
#8748=CARTESIAN_POINT('Ctrl Pts',(-6.63306845520281,15.3933171197393,7.));
#8749=CARTESIAN_POINT('Ctrl Pts',(-6.66297054550547,15.4424051151807,7.));
#8750=CARTESIAN_POINT('Ctrl Pts',(-6.68074830397731,15.4733031879166,7.));
#8751=CARTESIAN_POINT('Ctrl Pts',(-6.69953551835474,15.5083268912119,7.));
#8752=CARTESIAN_POINT('Ctrl Pts',(-6.72790031412628,15.5619248294191,7.));
#8753=CARTESIAN_POINT('Ctrl Pts',(-6.77211692048667,15.6387111659832,7.));
#8754=CARTESIAN_POINT('Ctrl Pts',(-6.83570676658072,15.7406883947778,7.));
#8755=CARTESIAN_POINT('Ctrl Pts',(-6.91534043556374,15.8583036897433,7.));
#8756=CARTESIAN_POINT('Ctrl Pts',(-7.01217619187967,15.9905219781863,7.));
#8757=CARTESIAN_POINT('Ctrl Pts',(-7.12742326811385,16.1361838672874,7.));
#8758=CARTESIAN_POINT('Ctrl Pts',(-7.26219165995682,16.2940809887434,7.));
#8759=CARTESIAN_POINT('Ctrl Pts',(-7.41753779118424,16.4629349257385,7.));
#8760=CARTESIAN_POINT('Ctrl Pts',(-7.59444470905137,16.6414085620714,7.));
#8761=CARTESIAN_POINT('Ctrl Pts',(-7.8457132052331,16.8766905033058,7.));
#8762=CARTESIAN_POINT('Ctrl Pts',(-8.04476736935674,17.0448123137865,7.));
#8763=CARTESIAN_POINT('Ctrl Pts',(-8.1773289360728,17.1502563092004,7.));
#8764=CARTESIAN_POINT('',(-9.06833546026097,16.6962658094609,7.));
#8765=CARTESIAN_POINT('Origin',(1.73472347597681E-15,0.,7.));
#8766=CARTESIAN_POINT('',(-8.68235805704666,13.7360532384392,7.));
#8767=CARTESIAN_POINT('Ctrl Pts',(-9.06833546026097,16.6962658094609,7.));
#8768=CARTESIAN_POINT('Ctrl Pts',(-9.06094720995302,16.5270428237395,7.));
#8769=CARTESIAN_POINT('Ctrl Pts',(-9.04193491022831,16.2671851013731,7.));
#8770=CARTESIAN_POINT('Ctrl Pts',(-8.9992797377215,15.9256093626227,7.));
#8771=CARTESIAN_POINT('Ctrl Pts',(-8.95887481023115,15.6775844882862,7.));
#8772=CARTESIAN_POINT('Ctrl Pts',(-8.91357927057119,15.4526569741556,7.));
#8773=CARTESIAN_POINT('Ctrl Pts',(-8.8650526891508,15.2508174554788,7.));
#8774=CARTESIAN_POINT('Ctrl Pts',(-8.81495027721559,15.0719627020186,7.));
#8775=CARTESIAN_POINT('Ctrl Pts',(-8.76490206435507,14.9159049694657,7.));
#8776=CARTESIAN_POINT('Ctrl Pts',(-8.71655678814369,14.7823474421093,7.));
#8777=CARTESIAN_POINT('Ctrl Pts',(-8.67143265073926,14.6709614647944,7.));
#8778=CARTESIAN_POINT('Ctrl Pts',(-8.63530106864816,14.5900556026053,7.));
#8779=CARTESIAN_POINT('Ctrl Pts',(-8.60861183441386,14.5356039231527,7.));
#8780=CARTESIAN_POINT('Ctrl Pts',(-8.59131991078476,14.4998183311667,7.));
#8781=CARTESIAN_POINT('Ctrl Pts',(-8.57677234909655,14.4672743909627,7.));
#8782=CARTESIAN_POINT('Ctrl Pts',(-8.55463533425729,14.4142298919554,7.));
#8783=CARTESIAN_POINT('Ctrl Pts',(-8.52826254822913,14.3397580968626,7.));
#8784=CARTESIAN_POINT('Ctrl Pts',(-8.50424841775454,14.2409143873564,7.));
#8785=CARTESIAN_POINT('Ctrl Pts',(-8.49286891019839,14.1356264252377,7.));
#8786=CARTESIAN_POINT('Ctrl Pts',(-8.50092900394916,14.0177193038531,7.));
#8787=CARTESIAN_POINT('Ctrl Pts',(-8.54836196063204,13.8694768008521,7.));
#8788=CARTESIAN_POINT('Ctrl Pts',(-8.62589941321477,13.7778907925313,7.));
#8789=CARTESIAN_POINT('Ctrl Pts',(-8.68235805704666,13.7360532384392,7.));
#8790=CARTESIAN_POINT('',(-10.380766749719,12.5020870932788,7.));
#8791=CARTESIAN_POINT('Origin',(0.,0.,7.));
#8792=CARTESIAN_POINT('',(-13.07682262797,13.7839294091566,7.));
#8793=CARTESIAN_POINT('Ctrl Pts',(-10.380766749719,12.5020870932788,7.));
#8794=CARTESIAN_POINT('Ctrl Pts',(-10.4380033085876,12.4613202473787,7.));
#8795=CARTESIAN_POINT('Ctrl Pts',(-10.5490671691512,12.4158793808611,7.));
#8796=CARTESIAN_POINT('Ctrl Pts',(-10.7047117573307,12.4165774110367,7.));
#8797=CARTESIAN_POINT('Ctrl Pts',(-10.8193387993863,12.4453471106187,7.));
#8798=CARTESIAN_POINT('Ctrl Pts',(-10.9159571406243,12.48870543503,7.));
#8799=CARTESIAN_POINT('Ctrl Pts',(-11.0025423202232,12.5420886163255,7.));
#8800=CARTESIAN_POINT('Ctrl Pts',(-11.0652195671547,12.5901836766158,7.));
#8801=CARTESIAN_POINT('Ctrl Pts',(-11.1088271697991,12.6276288804813,7.));
#8802=CARTESIAN_POINT('Ctrl Pts',(-11.1352828524077,12.651521064408,7.));
#8803=CARTESIAN_POINT('Ctrl Pts',(-11.1639734745886,12.6790250171322,7.));
#8804=CARTESIAN_POINT('Ctrl Pts',(-11.20751267221,12.7212344815888,7.));
#8805=CARTESIAN_POINT('Ctrl Pts',(-11.2732934467516,12.7805989445416,7.));
#8806=CARTESIAN_POINT('Ctrl Pts',(-11.3652836809863,12.8579347093876,7.));
#8807=CARTESIAN_POINT('Ctrl Pts',(-11.4773649257319,12.9451853450404,7.));
#8808=CARTESIAN_POINT('Ctrl Pts',(-11.6103189008826,13.0410085154727,7.));
#8809=CARTESIAN_POINT('Ctrl Pts',(-11.764937382884,13.1439278991698,7.));
#8810=CARTESIAN_POINT('Ctrl Pts',(-11.9419026340297,13.2524512620507,7.));
#8811=CARTESIAN_POINT('Ctrl Pts',(-12.1418243205134,13.3650363045724,7.));
#8812=CARTESIAN_POINT('Ctrl Pts',(-12.3652241842034,13.4801075753502,7.));
#8813=CARTESIAN_POINT('Ctrl Pts',(-12.6769008431476,13.6262277632565,7.));
#8814=CARTESIAN_POINT('Ctrl Pts',(-12.9181650995968,13.7246099871303,7.));
#8815=CARTESIAN_POINT('Ctrl Pts',(-13.07682262797,13.7839294091566,7.));
#8816=CARTESIAN_POINT('',(-13.7839294091564,13.0768226279702,7.));
#8817=CARTESIAN_POINT('Origin',(1.57723797680727E-16,0.,7.));
#8818=CARTESIAN_POINT('',(-12.5020870932787,10.3807667497191,7.));
#8819=CARTESIAN_POINT('Ctrl Pts',(-13.7839294091564,13.0768226279702,7.));
#8820=CARTESIAN_POINT('Ctrl Pts',(-13.7246099871302,12.9181650995968,7.));
#8821=CARTESIAN_POINT('Ctrl Pts',(-13.6262277632565,12.6769008431476,7.));
#8822=CARTESIAN_POINT('Ctrl Pts',(-13.4801075753502,12.3652241842034,7.));
#8823=CARTESIAN_POINT('Ctrl Pts',(-13.3650363045723,12.1418243205134,7.));
#8824=CARTESIAN_POINT('Ctrl Pts',(-13.2524512620508,11.9419026340297,7.));
#8825=CARTESIAN_POINT('Ctrl Pts',(-13.1439278991698,11.764937382884,7.));
#8826=CARTESIAN_POINT('Ctrl Pts',(-13.0410085154728,11.6103189008826,7.));
#8827=CARTESIAN_POINT('Ctrl Pts',(-12.9451853450404,11.4773649257318,7.));
#8828=CARTESIAN_POINT('Ctrl Pts',(-12.8579347093876,11.3652836809863,7.));
#8829=CARTESIAN_POINT('Ctrl Pts',(-12.7805989445416,11.2732934467516,7.));
#8830=CARTESIAN_POINT('Ctrl Pts',(-12.7212344815888,11.2075126722099,7.));
#8831=CARTESIAN_POINT('Ctrl Pts',(-12.6790250171322,11.1639734745886,7.));
#8832=CARTESIAN_POINT('Ctrl Pts',(-12.651521064408,11.1352828524077,7.));
#8833=CARTESIAN_POINT('Ctrl Pts',(-12.6276288804813,11.1088271697991,7.));
#8834=CARTESIAN_POINT('Ctrl Pts',(-12.5901836766158,11.0652195671547,7.));
#8835=CARTESIAN_POINT('Ctrl Pts',(-12.5420886163255,11.0025423202231,7.));
#8836=CARTESIAN_POINT('Ctrl Pts',(-12.48870543503,10.9159571406243,7.));
#8837=CARTESIAN_POINT('Ctrl Pts',(-12.4453471106187,10.8193387993863,7.));
#8838=CARTESIAN_POINT('Ctrl Pts',(-12.4165774110367,10.7047117573307,7.));
#8839=CARTESIAN_POINT('Ctrl Pts',(-12.4158793808611,10.5490671691512,7.));
#8840=CARTESIAN_POINT('Ctrl Pts',(-12.4613202473787,10.4380033085876,7.));
#8841=CARTESIAN_POINT('Ctrl Pts',(-12.5020870932787,10.3807667497191,7.));
#8842=CARTESIAN_POINT('',(-13.7360532384391,8.68235805704682,7.));
#8843=CARTESIAN_POINT('Origin',(0.,0.,7.));
#8844=CARTESIAN_POINT('',(-16.6962658094608,9.06833546026117,7.));
#8845=CARTESIAN_POINT('Ctrl Pts',(-13.7360532384391,8.68235805704682,7.));
#8846=CARTESIAN_POINT('Ctrl Pts',(-13.7778907925313,8.62589941321479,7.));
#8847=CARTESIAN_POINT('Ctrl Pts',(-13.8694768008521,8.54836196063206,7.));
#8848=CARTESIAN_POINT('Ctrl Pts',(-14.0177193038531,8.50092900394919,7.));
#8849=CARTESIAN_POINT('Ctrl Pts',(-14.1356264252377,8.49286891019842,7.));
#8850=CARTESIAN_POINT('Ctrl Pts',(-14.2409143873564,8.50424841775455,7.));
#8851=CARTESIAN_POINT('Ctrl Pts',(-14.3397580968626,8.52826254822914,7.));
#8852=CARTESIAN_POINT('Ctrl Pts',(-14.4142298919555,8.55463533425731,7.));
#8853=CARTESIAN_POINT('Ctrl Pts',(-14.4672743909627,8.57677234909655,7.));
#8854=CARTESIAN_POINT('Ctrl Pts',(-14.4998183311667,8.59131991078475,7.));
#8855=CARTESIAN_POINT('Ctrl Pts',(-14.5356039231527,8.60861183441388,7.));
#8856=CARTESIAN_POINT('Ctrl Pts',(-14.5900556026053,8.63530106864817,7.));
#8857=CARTESIAN_POINT('Ctrl Pts',(-14.6709614647944,8.67143265073926,7.));
#8858=CARTESIAN_POINT('Ctrl Pts',(-14.7823474421093,8.71655678814371,7.));
#8859=CARTESIAN_POINT('Ctrl Pts',(-14.9159049694657,8.76490206435508,7.));
#8860=CARTESIAN_POINT('Ctrl Pts',(-15.0719627020186,8.81495027721556,7.));
#8861=CARTESIAN_POINT('Ctrl Pts',(-15.2508174554788,8.86505268915083,7.));
#8862=CARTESIAN_POINT('Ctrl Pts',(-15.4526569741556,8.91357927057117,7.));
#8863=CARTESIAN_POINT('Ctrl Pts',(-15.6775844882863,8.95887481023116,7.));
#8864=CARTESIAN_POINT('Ctrl Pts',(-15.9256093626227,8.99927973772153,7.));
#8865=CARTESIAN_POINT('Ctrl Pts',(-16.2671851013731,9.04193491022832,7.));
#8866=CARTESIAN_POINT('Ctrl Pts',(-16.5270428237395,9.06094720995306,7.));
#8867=CARTESIAN_POINT('Ctrl Pts',(-16.6962658094608,9.06833546026117,7.));
#8868=CARTESIAN_POINT('',(-17.1502563092003,8.17732893607296,7.));
#8869=CARTESIAN_POINT('Origin',(-1.73472347597681E-15,0.,7.));
#8870=CARTESIAN_POINT('',(-15.0980247376578,6.00933848448163,7.));
#8871=CARTESIAN_POINT('Ctrl Pts',(-17.1502563092003,8.17732893607296,7.));
#8872=CARTESIAN_POINT('Ctrl Pts',(-17.0448123137865,8.04476736935675,7.));
#8873=CARTESIAN_POINT('Ctrl Pts',(-16.8766905033057,7.8457132052331,7.));
#8874=CARTESIAN_POINT('Ctrl Pts',(-16.6414085620714,7.59444470905138,7.));
#8875=CARTESIAN_POINT('Ctrl Pts',(-16.4629349257385,7.41753779118423,7.));
#8876=CARTESIAN_POINT('Ctrl Pts',(-16.2940809887434,7.26219165995682,7.));
#8877=CARTESIAN_POINT('Ctrl Pts',(-16.1361838672874,7.12742326811386,7.));
#8878=CARTESIAN_POINT('Ctrl Pts',(-15.9905219781863,7.01217619187965,7.));
#8879=CARTESIAN_POINT('Ctrl Pts',(-15.8583036897432,6.91534043556372,7.));
#8880=CARTESIAN_POINT('Ctrl Pts',(-15.7406883947777,6.83570676658073,7.));
#8881=CARTESIAN_POINT('Ctrl Pts',(-15.6387111659832,6.77211692048666,7.));
#8882=CARTESIAN_POINT('Ctrl Pts',(-15.5619248294191,6.72790031412627,7.));
#8883=CARTESIAN_POINT('Ctrl Pts',(-15.5083268912118,6.69953551835476,7.));
#8884=CARTESIAN_POINT('Ctrl Pts',(-15.4733031879166,6.68074830397729,7.));
#8885=CARTESIAN_POINT('Ctrl Pts',(-15.4424051151807,6.66297054550545,7.));
#8886=CARTESIAN_POINT('Ctrl Pts',(-15.3933171197393,6.6330684552028,7.));
#8887=CARTESIAN_POINT('Ctrl Pts',(-15.3282076647861,6.58832104206026,7.));
#8888=CARTESIAN_POINT('Ctrl Pts',(-15.2506809503975,6.5224699530223,7.));
#8889=CARTESIAN_POINT('Ctrl Pts',(-15.1795880240196,6.443978909085,7.));
#8890=CARTESIAN_POINT('Ctrl Pts',(-15.1168047097501,6.34385243988827,7.));
#8891=CARTESIAN_POINT('Ctrl Pts',(-15.0680440207731,6.19604134326095,7.));
#8892=CARTESIAN_POINT('Ctrl Pts',(-15.0769402326058,6.07637133495398,7.));
#8893=CARTESIAN_POINT('Ctrl Pts',(-15.0980247376578,6.00933848448163,7.));
#8894=CARTESIAN_POINT('',(-15.7467591314704,4.01273932064536,7.));
#8895=CARTESIAN_POINT('Origin',(0.,0.,7.));
#8896=CARTESIAN_POINT('',(-18.6813621637973,3.46506965370702,7.));
#8897=CARTESIAN_POINT('Ctrl Pts',(-15.7467591314704,4.01273932064536,7.));
#8898=CARTESIAN_POINT('Ctrl Pts',(-15.7691023294921,3.94611544431018,7.));
#8899=CARTESIAN_POINT('Ctrl Pts',(-15.8322454089585,3.84407131175636,7.));
#8900=CARTESIAN_POINT('Ctrl Pts',(-15.958574817721,3.75315043649999,7.));
#8901=CARTESIAN_POINT('Ctrl Pts',(-16.0682204478862,3.7090495275507,7.));
#8902=CARTESIAN_POINT('Ctrl Pts',(-16.1718717115691,3.68733631276638,7.));
#8903=CARTESIAN_POINT('Ctrl Pts',(-16.2732984400115,3.67963072201295,7.));
#8904=CARTESIAN_POINT('Ctrl Pts',(-16.3522749650865,3.68169968173258,7.));
#8905=CARTESIAN_POINT('Ctrl Pts',(-16.409563995311,3.68636158229543,7.));
#8906=CARTESIAN_POINT('Ctrl Pts',(-16.4450105654964,3.69014050504823,7.));
#8907=CARTESIAN_POINT('Ctrl Pts',(-16.4843881842109,3.69552774561757,7.));
#8908=CARTESIAN_POINT('Ctrl Pts',(-16.5444222357228,3.70408422142789,7.));
#8909=CARTESIAN_POINT('Ctrl Pts',(-16.632533556064,3.7134461116587,7.));
#8910=CARTESIAN_POINT('Ctrl Pts',(-16.7524120409277,3.72194155665404,7.));
#8911=CARTESIAN_POINT('Ctrl Pts',(-16.8943723095674,3.72664910094711,7.));
#8912=CARTESIAN_POINT('Ctrl Pts',(-17.0582577813421,3.72602328845453,7.));
#8913=CARTESIAN_POINT('Ctrl Pts',(-17.2438412568379,3.71840435546374,7.));
#8914=CARTESIAN_POINT('Ctrl Pts',(-17.4507975846592,3.70218403552947,7.));
#8915=CARTESIAN_POINT('Ctrl Pts',(-17.6787134541915,3.67575622931334,7.));
#8916=CARTESIAN_POINT('Ctrl Pts',(-17.9270849363835,3.63753969769581,7.));
#8917=CARTESIAN_POINT('Ctrl Pts',(-18.265123941733,3.57255446932205,7.));
#8918=CARTESIAN_POINT('Ctrl Pts',(-18.5181384456163,3.51033578853423,7.));
#8919=CARTESIAN_POINT('Ctrl Pts',(-18.6813621637973,3.46506965370702,7.));
#8920=CARTESIAN_POINT('',(-18.8377966288375,2.47738131311205,7.));
#8921=CARTESIAN_POINT('Origin',(0.,0.,7.));
#8922=CARTESIAN_POINT('Ctrl Pts',(-18.8377966288375,2.47738131311205,7.));
#8923=CARTESIAN_POINT('Ctrl Pts',(-18.6965496529788,2.38389175781397,7.));
#8924=CARTESIAN_POINT('Ctrl Pts',(-18.4751451900744,2.24653249449212,7.));
#8925=CARTESIAN_POINT('Ctrl Pts',(-18.1737325312257,2.08026807216975,7.));
#8926=CARTESIAN_POINT('Ctrl Pts',(-17.949326772361,1.96717098182926,7.));
#8927=CARTESIAN_POINT('Ctrl Pts',(-17.7407325407201,1.87160676754277,7.));
#8928=CARTESIAN_POINT('Ctrl Pts',(-17.548917731071,1.79222730418272,7.));
#8929=CARTESIAN_POINT('Ctrl Pts',(-17.3747717371572,1.72763282051119,7.));
#8930=CARTESIAN_POINT('Ctrl Pts',(-17.2191007779952,1.67639424155264,7.));
#8931=CARTESIAN_POINT('Ctrl Pts',(-17.0826338282621,1.63700324669263,7.));
#8932=CARTESIAN_POINT('Ctrl Pts',(-16.9659973771906,1.60803840593145,7.));
#8933=CARTESIAN_POINT('Ctrl Pts',(-16.8793055486399,1.58971419725805,7.));
#8934=CARTESIAN_POINT('Ctrl Pts',(-16.8195656763126,1.57930034717566,7.));
#8935=CARTESIAN_POINT('Ctrl Pts',(-16.7804505865492,1.57225556404312,7.));
#8936=CARTESIAN_POINT('Ctrl Pts',(-16.7455711436431,1.56489594057218,7.));
#8937=CARTESIAN_POINT('Ctrl Pts',(-16.6896454316358,1.55162638755017,7.));
#8938=CARTESIAN_POINT('Ctrl Pts',(-16.6138949491149,1.52918899676863,7.));
#8939=CARTESIAN_POINT('Ctrl Pts',(-16.5198135565977,1.4905179616981,7.));
#8940=CARTESIAN_POINT('Ctrl Pts',(-16.4279450992207,1.43783746532133,7.));
#8941=CARTESIAN_POINT('Ctrl Pts',(-16.3372938385016,1.3620126454106,7.));
#8942=CARTESIAN_POINT('Ctrl Pts',(-16.2452435266959,1.23650382033378,7.));
#8943=CARTESIAN_POINT('Ctrl Pts',(-16.2167242606458,1.1199417984865,7.));
#8944=CARTESIAN_POINT('Ctrl Pts',(-16.2160625265911,1.04967429885986,7.));
#8945=CARTESIAN_POINT('',(-18.8377966288376,-2.47738131311187,7.));
#8946=CARTESIAN_POINT('Ctrl Pts',(-16.2160625265912,-1.04967429885971,7.));
#8947=CARTESIAN_POINT('Ctrl Pts',(-16.2167242606459,-1.11994179848649,7.));
#8948=CARTESIAN_POINT('Ctrl Pts',(-16.2452435266959,-1.23650382033376,7.));
#8949=CARTESIAN_POINT('Ctrl Pts',(-16.3372938385016,-1.36201264541056,7.));
#8950=CARTESIAN_POINT('Ctrl Pts',(-16.4279450992208,-1.43783746532131,7.));
#8951=CARTESIAN_POINT('Ctrl Pts',(-16.5198135565978,-1.49051796169811,7.));
#8952=CARTESIAN_POINT('Ctrl Pts',(-16.6138949491149,-1.52918899676863,7.));
#8953=CARTESIAN_POINT('Ctrl Pts',(-16.6896454316359,-1.55162638755017,7.));
#8954=CARTESIAN_POINT('Ctrl Pts',(-16.7455711436431,-1.56489594057219,7.));
#8955=CARTESIAN_POINT('Ctrl Pts',(-16.7804505865492,-1.57225556404312,7.));
#8956=CARTESIAN_POINT('Ctrl Pts',(-16.8195656763126,-1.57930034717562,7.));
#8957=CARTESIAN_POINT('Ctrl Pts',(-16.8793055486399,-1.58971419725805,7.));
#8958=CARTESIAN_POINT('Ctrl Pts',(-16.9659973771906,-1.60803840593145,7.));
#8959=CARTESIAN_POINT('Ctrl Pts',(-17.0826338282621,-1.63700324669261,7.));
#8960=CARTESIAN_POINT('Ctrl Pts',(-17.2191007779953,-1.67639424155264,7.));
#8961=CARTESIAN_POINT('Ctrl Pts',(-17.3747717371572,-1.72763282051121,7.));
#8962=CARTESIAN_POINT('Ctrl Pts',(-17.548917731071,-1.79222730418269,7.));
#8963=CARTESIAN_POINT('Ctrl Pts',(-17.7407325407201,-1.87160676754278,7.));
#8964=CARTESIAN_POINT('Ctrl Pts',(-17.949326772361,-1.96717098182925,7.));
#8965=CARTESIAN_POINT('Ctrl Pts',(-18.1737325312258,-2.08026807216972,7.));
#8966=CARTESIAN_POINT('Ctrl Pts',(-18.4751451900744,-2.2465324944921,7.));
#8967=CARTESIAN_POINT('Ctrl Pts',(-18.6965496529788,-2.38389175781394,7.));
#8968=CARTESIAN_POINT('Ctrl Pts',(-18.8377966288376,-2.47738131311187,7.));
#8969=CARTESIAN_POINT('',(-18.6813621637974,-3.46506965370684,7.));
#8970=CARTESIAN_POINT('Origin',(0.,0.,7.));
#8971=CARTESIAN_POINT('',(-15.7467591314705,-4.0127393206452,7.));
#8972=CARTESIAN_POINT('Ctrl Pts',(-18.6813621637974,-3.46506965370684,7.));
#8973=CARTESIAN_POINT('Ctrl Pts',(-18.5181384456162,-3.51033578853419,7.));
#8974=CARTESIAN_POINT('Ctrl Pts',(-18.265123941733,-3.57255446932203,7.));
#8975=CARTESIAN_POINT('Ctrl Pts',(-17.9270849363835,-3.63753969769578,7.));
#8976=CARTESIAN_POINT('Ctrl Pts',(-17.6787134541915,-3.67575622931333,7.));
#8977=CARTESIAN_POINT('Ctrl Pts',(-17.4507975846592,-3.70218403552949,7.));
#8978=CARTESIAN_POINT('Ctrl Pts',(-17.2438412568379,-3.71840435546371,7.));
#8979=CARTESIAN_POINT('Ctrl Pts',(-17.0582577813421,-3.72602328845455,7.));
#8980=CARTESIAN_POINT('Ctrl Pts',(-16.8943723095674,-3.7266491009471,7.));
#8981=CARTESIAN_POINT('Ctrl Pts',(-16.7524120409277,-3.72194155665402,7.));
#8982=CARTESIAN_POINT('Ctrl Pts',(-16.632533556064,-3.7134461116587,7.));
#8983=CARTESIAN_POINT('Ctrl Pts',(-16.5444222357228,-3.70408422142789,7.));
#8984=CARTESIAN_POINT('Ctrl Pts',(-16.4843881842109,-3.69552774561754,7.));
#8985=CARTESIAN_POINT('Ctrl Pts',(-16.4450105654964,-3.69014050504824,7.));
#8986=CARTESIAN_POINT('Ctrl Pts',(-16.409563995311,-3.68636158229544,7.));
#8987=CARTESIAN_POINT('Ctrl Pts',(-16.3522749650865,-3.68169968173258,7.));
#8988=CARTESIAN_POINT('Ctrl Pts',(-16.2732984400115,-3.67963072201294,7.));
#8989=CARTESIAN_POINT('Ctrl Pts',(-16.1718717115691,-3.68733631276639,7.));
#8990=CARTESIAN_POINT('Ctrl Pts',(-16.0682204478862,-3.70904952755068,7.));
#8991=CARTESIAN_POINT('Ctrl Pts',(-15.958574817721,-3.75315043649995,7.));
#8992=CARTESIAN_POINT('Ctrl Pts',(-15.8322454089585,-3.84407131175635,7.));
#8993=CARTESIAN_POINT('Ctrl Pts',(-15.7691023294921,-3.94611544431017,7.));
#8994=CARTESIAN_POINT('Ctrl Pts',(-15.7467591314705,-4.0127393206452,7.));
#8995=CARTESIAN_POINT('',(-15.0980247376579,-6.00933848448149,7.));
#8996=CARTESIAN_POINT('Origin',(0.,0.,7.));
#8997=CARTESIAN_POINT('',(-17.1502563092004,-8.1773289360728,7.));
#8998=CARTESIAN_POINT('Ctrl Pts',(-15.0980247376579,-6.00933848448149,7.));
#8999=CARTESIAN_POINT('Ctrl Pts',(-15.0769402326058,-6.07637133495397,7.));
#9000=CARTESIAN_POINT('Ctrl Pts',(-15.0680440207731,-6.19604134326091,7.));
#9001=CARTESIAN_POINT('Ctrl Pts',(-15.1168047097502,-6.34385243988823,7.));
#9002=CARTESIAN_POINT('Ctrl Pts',(-15.1795880240196,-6.44397890908498,7.));
#9003=CARTESIAN_POINT('Ctrl Pts',(-15.2506809503975,-6.52246995302231,7.));
#9004=CARTESIAN_POINT('Ctrl Pts',(-15.3282076647862,-6.58832104206025,7.));
#9005=CARTESIAN_POINT('Ctrl Pts',(-15.3933171197393,-6.63306845520279,7.));
#9006=CARTESIAN_POINT('Ctrl Pts',(-15.4424051151807,-6.66297054550545,7.));
#9007=CARTESIAN_POINT('Ctrl Pts',(-15.4733031879166,-6.68074830397729,7.));
#9008=CARTESIAN_POINT('Ctrl Pts',(-15.5083268912119,-6.69953551835472,7.));
#9009=CARTESIAN_POINT('Ctrl Pts',(-15.5619248294191,-6.72790031412626,7.));
#9010=CARTESIAN_POINT('Ctrl Pts',(-15.6387111659832,-6.77211692048665,7.));
#9011=CARTESIAN_POINT('Ctrl Pts',(-15.7406883947778,-6.8357067665807,7.));
#9012=CARTESIAN_POINT('Ctrl Pts',(-15.8583036897433,-6.91534043556372,7.));
#9013=CARTESIAN_POINT('Ctrl Pts',(-15.9905219781863,-7.01217619187965,7.));
#9014=CARTESIAN_POINT('Ctrl Pts',(-16.1361838672874,-7.12742326811382,7.));
#9015=CARTESIAN_POINT('Ctrl Pts',(-16.2940809887434,-7.26219165995681,7.));
#9016=CARTESIAN_POINT('Ctrl Pts',(-16.4629349257385,-7.41753779118423,7.));
#9017=CARTESIAN_POINT('Ctrl Pts',(-16.6414085620714,-7.59444470905136,7.));
#9018=CARTESIAN_POINT('Ctrl Pts',(-16.8766905033058,-7.84571320523309,7.));
#9019=CARTESIAN_POINT('Ctrl Pts',(-17.0448123137865,-8.04476736935674,7.));
#9020=CARTESIAN_POINT('Ctrl Pts',(-17.1502563092004,-8.1773289360728,7.));
#9021=CARTESIAN_POINT('',(-16.6962658094609,-9.06833546026103,7.));
#9022=CARTESIAN_POINT('Origin',(0.,0.,7.));
#9023=CARTESIAN_POINT('',(-13.7360532384392,-8.68235805704666,7.));
#9024=CARTESIAN_POINT('Ctrl Pts',(-16.6962658094609,-9.06833546026103,7.));
#9025=CARTESIAN_POINT('Ctrl Pts',(-16.5270428237395,-9.06094720995301,7.));
#9026=CARTESIAN_POINT('Ctrl Pts',(-16.2671851013731,-9.0419349102283,7.));
#9027=CARTESIAN_POINT('Ctrl Pts',(-15.9256093626227,-8.99927973772149,7.));
#9028=CARTESIAN_POINT('Ctrl Pts',(-15.6775844882862,-8.95887481023114,7.));
#9029=CARTESIAN_POINT('Ctrl Pts',(-15.4526569741556,-8.91357927057118,7.));
#9030=CARTESIAN_POINT('Ctrl Pts',(-15.2508174554788,-8.8650526891508,7.));
#9031=CARTESIAN_POINT('Ctrl Pts',(-15.0719627020186,-8.81495027721558,7.));
#9032=CARTESIAN_POINT('Ctrl Pts',(-14.9159049694657,-8.76490206435507,7.));
#9033=CARTESIAN_POINT('Ctrl Pts',(-14.7823474421093,-8.71655678814369,7.));
#9034=CARTESIAN_POINT('Ctrl Pts',(-14.6709614647944,-8.67143265073926,7.));
#9035=CARTESIAN_POINT('Ctrl Pts',(-14.5900556026053,-8.63530106864816,7.));
#9036=CARTESIAN_POINT('Ctrl Pts',(-14.5356039231527,-8.60861183441385,7.));
#9037=CARTESIAN_POINT('Ctrl Pts',(-14.4998183311667,-8.59131991078476,7.));
#9038=CARTESIAN_POINT('Ctrl Pts',(-14.4672743909627,-8.57677234909656,7.));
#9039=CARTESIAN_POINT('Ctrl Pts',(-14.4142298919554,-8.5546353342573,7.));
#9040=CARTESIAN_POINT('Ctrl Pts',(-14.3397580968625,-8.52826254822913,7.));
#9041=CARTESIAN_POINT('Ctrl Pts',(-14.2409143873564,-8.50424841775454,7.));
#9042=CARTESIAN_POINT('Ctrl Pts',(-14.1356264252376,-8.4928689101984,7.));
#9043=CARTESIAN_POINT('Ctrl Pts',(-14.0177193038531,-8.50092900394916,7.));
#9044=CARTESIAN_POINT('Ctrl Pts',(-13.8694768008521,-8.54836196063206,7.));
#9045=CARTESIAN_POINT('Ctrl Pts',(-13.7778907925313,-8.62589941321478,7.));
#9046=CARTESIAN_POINT('Ctrl Pts',(-13.7360532384392,-8.68235805704666,7.));
#9047=CARTESIAN_POINT('',(-12.5020870932788,-10.380766749719,7.));
#9048=CARTESIAN_POINT('Origin',(0.,0.,7.));
#9049=CARTESIAN_POINT('',(-13.7839294091566,-13.07682262797,7.));
#9050=CARTESIAN_POINT('Ctrl Pts',(-12.5020870932788,-10.380766749719,7.));
#9051=CARTESIAN_POINT('Ctrl Pts',(-12.4613202473788,-10.4380033085876,7.));
#9052=CARTESIAN_POINT('Ctrl Pts',(-12.4158793808611,-10.5490671691512,7.));
#9053=CARTESIAN_POINT('Ctrl Pts',(-12.4165774110367,-10.7047117573306,7.));
#9054=CARTESIAN_POINT('Ctrl Pts',(-12.4453471106188,-10.8193387993863,7.));
#9055=CARTESIAN_POINT('Ctrl Pts',(-12.4887054350301,-10.9159571406243,7.));
#9056=CARTESIAN_POINT('Ctrl Pts',(-12.5420886163255,-11.0025423202231,7.));
#9057=CARTESIAN_POINT('Ctrl Pts',(-12.5901836766158,-11.0652195671547,7.));
#9058=CARTESIAN_POINT('Ctrl Pts',(-12.6276288804813,-11.1088271697991,7.));
#9059=CARTESIAN_POINT('Ctrl Pts',(-12.6515210644081,-11.1352828524077,7.));
#9060=CARTESIAN_POINT('Ctrl Pts',(-12.6790250171322,-11.1639734745885,7.));
#9061=CARTESIAN_POINT('Ctrl Pts',(-12.7212344815888,-11.2075126722099,7.));
#9062=CARTESIAN_POINT('Ctrl Pts',(-12.7805989445416,-11.2732934467515,7.));
#9063=CARTESIAN_POINT('Ctrl Pts',(-12.8579347093876,-11.3652836809863,7.));
#9064=CARTESIAN_POINT('Ctrl Pts',(-12.9451853450404,-11.4773649257318,7.));
#9065=CARTESIAN_POINT('Ctrl Pts',(-13.0410085154727,-11.6103189008825,7.));
#9066=CARTESIAN_POINT('Ctrl Pts',(-13.1439278991698,-11.764937382884,7.));
#9067=CARTESIAN_POINT('Ctrl Pts',(-13.2524512620508,-11.9419026340297,7.));
#9068=CARTESIAN_POINT('Ctrl Pts',(-13.3650363045724,-12.1418243205134,7.));
#9069=CARTESIAN_POINT('Ctrl Pts',(-13.4801075753502,-12.3652241842034,7.));
#9070=CARTESIAN_POINT('Ctrl Pts',(-13.6262277632565,-12.6769008431476,7.));
#9071=CARTESIAN_POINT('Ctrl Pts',(-13.7246099871303,-12.9181650995967,7.));
#9072=CARTESIAN_POINT('Ctrl Pts',(-13.7839294091566,-13.07682262797,7.));
#9073=CARTESIAN_POINT('',(-13.0768226279701,-13.7839294091565,7.));
#9074=CARTESIAN_POINT('Origin',(0.,0.,7.));
#9075=CARTESIAN_POINT('',(-10.3807667497191,-12.5020870932787,7.));
#9076=CARTESIAN_POINT('Ctrl Pts',(-13.0768226279701,-13.7839294091565,7.));
#9077=CARTESIAN_POINT('Ctrl Pts',(-12.9181650995967,-13.7246099871302,7.));
#9078=CARTESIAN_POINT('Ctrl Pts',(-12.6769008431476,-13.6262277632565,7.));
#9079=CARTESIAN_POINT('Ctrl Pts',(-12.3652241842034,-13.4801075753502,7.));
#9080=CARTESIAN_POINT('Ctrl Pts',(-12.1418243205134,-13.3650363045723,7.));
#9081=CARTESIAN_POINT('Ctrl Pts',(-11.9419026340297,-13.2524512620508,7.));
#9082=CARTESIAN_POINT('Ctrl Pts',(-11.764937382884,-13.1439278991698,7.));
#9083=CARTESIAN_POINT('Ctrl Pts',(-11.6103189008825,-13.0410085154728,7.));
#9084=CARTESIAN_POINT('Ctrl Pts',(-11.4773649257318,-12.9451853450404,7.));
#9085=CARTESIAN_POINT('Ctrl Pts',(-11.3652836809863,-12.8579347093876,7.));
#9086=CARTESIAN_POINT('Ctrl Pts',(-11.2732934467515,-12.7805989445416,7.));
#9087=CARTESIAN_POINT('Ctrl Pts',(-11.2075126722099,-12.7212344815888,7.));
#9088=CARTESIAN_POINT('Ctrl Pts',(-11.1639734745886,-12.6790250171322,7.));
#9089=CARTESIAN_POINT('Ctrl Pts',(-11.1352828524077,-12.651521064408,7.));
#9090=CARTESIAN_POINT('Ctrl Pts',(-11.1088271697991,-12.6276288804813,7.));
#9091=CARTESIAN_POINT('Ctrl Pts',(-11.0652195671547,-12.5901836766158,7.));
#9092=CARTESIAN_POINT('Ctrl Pts',(-11.0025423202231,-12.5420886163255,7.));
#9093=CARTESIAN_POINT('Ctrl Pts',(-10.9159571406243,-12.48870543503,7.));
#9094=CARTESIAN_POINT('Ctrl Pts',(-10.8193387993863,-12.4453471106187,7.));
#9095=CARTESIAN_POINT('Ctrl Pts',(-10.7047117573307,-12.4165774110367,7.));
#9096=CARTESIAN_POINT('Ctrl Pts',(-10.5490671691512,-12.4158793808611,7.));
#9097=CARTESIAN_POINT('Ctrl Pts',(-10.4380033085876,-12.4613202473787,7.));
#9098=CARTESIAN_POINT('Ctrl Pts',(-10.3807667497191,-12.5020870932787,7.));
#9099=CARTESIAN_POINT('',(-8.68235805704677,-13.7360532384392,7.));
#9100=CARTESIAN_POINT('Origin',(0.,0.,7.));
#9101=CARTESIAN_POINT('',(-9.06833546026116,-16.6962658094608,7.));
#9102=CARTESIAN_POINT('Ctrl Pts',(-8.68235805704677,-13.7360532384392,7.));
#9103=CARTESIAN_POINT('Ctrl Pts',(-8.62589941321481,-13.7778907925313,7.));
#9104=CARTESIAN_POINT('Ctrl Pts',(-8.54836196063208,-13.8694768008521,7.));
#9105=CARTESIAN_POINT('Ctrl Pts',(-8.50092900394921,-14.0177193038531,7.));
#9106=CARTESIAN_POINT('Ctrl Pts',(-8.49286891019844,-14.1356264252377,7.));
#9107=CARTESIAN_POINT('Ctrl Pts',(-8.50424841775456,-14.2409143873564,7.));
#9108=CARTESIAN_POINT('Ctrl Pts',(-8.52826254822915,-14.3397580968626,7.));
#9109=CARTESIAN_POINT('Ctrl Pts',(-8.55463533425732,-14.4142298919555,7.));
#9110=CARTESIAN_POINT('Ctrl Pts',(-8.57677234909656,-14.4672743909627,7.));
#9111=CARTESIAN_POINT('Ctrl Pts',(-8.59131991078476,-14.4998183311667,7.));
#9112=CARTESIAN_POINT('Ctrl Pts',(-8.6086118344139,-14.5356039231527,7.));
#9113=CARTESIAN_POINT('Ctrl Pts',(-8.63530106864818,-14.5900556026053,7.));
#9114=CARTESIAN_POINT('Ctrl Pts',(-8.67143265073928,-14.6709614647944,7.));
#9115=CARTESIAN_POINT('Ctrl Pts',(-8.71655678814373,-14.7823474421093,7.));
#9116=CARTESIAN_POINT('Ctrl Pts',(-8.76490206435509,-14.9159049694657,7.));
#9117=CARTESIAN_POINT('Ctrl Pts',(-8.81495027721557,-15.0719627020186,7.));
#9118=CARTESIAN_POINT('Ctrl Pts',(-8.86505268915084,-15.2508174554788,7.));
#9119=CARTESIAN_POINT('Ctrl Pts',(-8.91357927057117,-15.4526569741556,7.));
#9120=CARTESIAN_POINT('Ctrl Pts',(-8.95887481023116,-15.6775844882862,7.));
#9121=CARTESIAN_POINT('Ctrl Pts',(-8.99927973772154,-15.9256093626227,7.));
#9122=CARTESIAN_POINT('Ctrl Pts',(-9.04193491022832,-16.2671851013731,7.));
#9123=CARTESIAN_POINT('Ctrl Pts',(-9.06094720995306,-16.5270428237395,7.));
#9124=CARTESIAN_POINT('Ctrl Pts',(-9.06833546026116,-16.6962658094608,7.));
#9125=CARTESIAN_POINT('',(-8.17732893607292,-17.1502563092003,7.));
#9126=CARTESIAN_POINT('Origin',(0.,0.,7.));
#9127=CARTESIAN_POINT('',(-6.0093384844816,-15.0980247376578,7.));
#9128=CARTESIAN_POINT('Ctrl Pts',(-8.17732893607292,-17.1502563092003,7.));
#9129=CARTESIAN_POINT('Ctrl Pts',(-8.04476736935674,-17.0448123137865,7.));
#9130=CARTESIAN_POINT('Ctrl Pts',(-7.8457132052331,-16.8766905033057,7.));
#9131=CARTESIAN_POINT('Ctrl Pts',(-7.59444470905137,-16.6414085620714,7.));
#9132=CARTESIAN_POINT('Ctrl Pts',(-7.41753779118422,-16.4629349257385,7.));
#9133=CARTESIAN_POINT('Ctrl Pts',(-7.2621916599568,-16.2940809887434,7.));
#9134=CARTESIAN_POINT('Ctrl Pts',(-7.12742326811384,-16.1361838672874,7.));
#9135=CARTESIAN_POINT('Ctrl Pts',(-7.01217619187963,-15.9905219781863,7.));
#9136=CARTESIAN_POINT('Ctrl Pts',(-6.9153404355637,-15.8583036897432,7.));
#9137=CARTESIAN_POINT('Ctrl Pts',(-6.8357067665807,-15.7406883947777,7.));
#9138=CARTESIAN_POINT('Ctrl Pts',(-6.77211692048664,-15.6387111659832,7.));
#9139=CARTESIAN_POINT('Ctrl Pts',(-6.72790031412625,-15.5619248294191,7.));
#9140=CARTESIAN_POINT('Ctrl Pts',(-6.69953551835473,-15.5083268912118,7.));
#9141=CARTESIAN_POINT('Ctrl Pts',(-6.68074830397727,-15.4733031879166,7.));
#9142=CARTESIAN_POINT('Ctrl Pts',(-6.66297054550543,-15.4424051151807,7.));
#9143=CARTESIAN_POINT('Ctrl Pts',(-6.63306845520277,-15.3933171197393,7.));
#9144=CARTESIAN_POINT('Ctrl Pts',(-6.58832104206024,-15.3282076647861,7.));
#9145=CARTESIAN_POINT('Ctrl Pts',(-6.52246995302227,-15.2506809503975,7.));
#9146=CARTESIAN_POINT('Ctrl Pts',(-6.44397890908497,-15.1795880240196,7.));
#9147=CARTESIAN_POINT('Ctrl Pts',(-6.34385243988824,-15.1168047097501,7.));
#9148=CARTESIAN_POINT('Ctrl Pts',(-6.19604134326091,-15.0680440207731,7.));
#9149=CARTESIAN_POINT('Ctrl Pts',(-6.07637133495395,-15.0769402326058,7.));
#9150=CARTESIAN_POINT('Ctrl Pts',(-6.0093384844816,-15.0980247376578,7.));
#9151=CARTESIAN_POINT('',(-4.01273932064531,-15.7467591314704,7.));
#9152=CARTESIAN_POINT('Origin',(0.,0.,7.));
#9153=CARTESIAN_POINT('',(-3.46506965370701,-18.6813621637973,7.));
#9154=CARTESIAN_POINT('Ctrl Pts',(-4.01273932064531,-15.7467591314704,7.));
#9155=CARTESIAN_POINT('Ctrl Pts',(-3.94611544431022,-15.7691023294921,7.));
#9156=CARTESIAN_POINT('Ctrl Pts',(-3.8440713117564,-15.8322454089585,7.));
#9157=CARTESIAN_POINT('Ctrl Pts',(-3.75315043650002,-15.958574817721,7.));
#9158=CARTESIAN_POINT('Ctrl Pts',(-3.70904952755073,-16.0682204478862,7.));
#9159=CARTESIAN_POINT('Ctrl Pts',(-3.68733631276642,-16.1718717115691,7.));
#9160=CARTESIAN_POINT('Ctrl Pts',(-3.67963072201298,-16.2732984400115,7.));
#9161=CARTESIAN_POINT('Ctrl Pts',(-3.68169968173261,-16.3522749650865,7.));
#9162=CARTESIAN_POINT('Ctrl Pts',(-3.68636158229546,-16.409563995311,7.));
#9163=CARTESIAN_POINT('Ctrl Pts',(-3.69014050504826,-16.4450105654963,7.));
#9164=CARTESIAN_POINT('Ctrl Pts',(-3.6955277456176,-16.4843881842109,7.));
#9165=CARTESIAN_POINT('Ctrl Pts',(-3.70408422142792,-16.5444222357228,7.));
#9166=CARTESIAN_POINT('Ctrl Pts',(-3.71344611165872,-16.632533556064,7.));
#9167=CARTESIAN_POINT('Ctrl Pts',(-3.72194155665407,-16.7524120409277,7.));
#9168=CARTESIAN_POINT('Ctrl Pts',(-3.72664910094713,-16.8943723095674,7.));
#9169=CARTESIAN_POINT('Ctrl Pts',(-3.72602328845455,-17.0582577813421,7.));
#9170=CARTESIAN_POINT('Ctrl Pts',(-3.71840435546375,-17.2438412568379,7.));
#9171=CARTESIAN_POINT('Ctrl Pts',(-3.70218403552949,-17.4507975846592,7.));
#9172=CARTESIAN_POINT('Ctrl Pts',(-3.67575622931335,-17.6787134541915,7.));
#9173=CARTESIAN_POINT('Ctrl Pts',(-3.63753969769582,-17.9270849363835,7.));
#9174=CARTESIAN_POINT('Ctrl Pts',(-3.57255446932205,-18.265123941733,7.));
#9175=CARTESIAN_POINT('Ctrl Pts',(-3.51033578853422,-18.5181384456163,7.));
#9176=CARTESIAN_POINT('Ctrl Pts',(-3.46506965370701,-18.6813621637973,7.));
#9177=CARTESIAN_POINT('',(-2.47738131311198,-18.8377966288376,7.));
#9178=CARTESIAN_POINT('Origin',(0.,0.,7.));
#9179=CARTESIAN_POINT('',(-1.04967429885986,-16.2160625265911,7.));
#9180=CARTESIAN_POINT('Ctrl Pts',(-2.47738131311198,-18.8377966288376,7.));
#9181=CARTESIAN_POINT('Ctrl Pts',(-2.38389175781398,-18.6965496529788,7.));
#9182=CARTESIAN_POINT('Ctrl Pts',(-2.24653249449213,-18.4751451900744,7.));
#9183=CARTESIAN_POINT('Ctrl Pts',(-2.08026807216976,-18.1737325312257,7.));
#9184=CARTESIAN_POINT('Ctrl Pts',(-1.96717098182926,-17.949326772361,7.));
#9185=CARTESIAN_POINT('Ctrl Pts',(-1.87160676754278,-17.7407325407201,7.));
#9186=CARTESIAN_POINT('Ctrl Pts',(-1.79222730418273,-17.548917731071,7.));
#9187=CARTESIAN_POINT('Ctrl Pts',(-1.7276328205112,-17.3747717371572,7.));
#9188=CARTESIAN_POINT('Ctrl Pts',(-1.67639424155264,-17.2191007779952,7.));
#9189=CARTESIAN_POINT('Ctrl Pts',(-1.63700324669264,-17.0826338282621,7.));
#9190=CARTESIAN_POINT('Ctrl Pts',(-1.60803840593146,-16.9659973771906,7.));
#9191=CARTESIAN_POINT('Ctrl Pts',(-1.58971419725806,-16.8793055486399,7.));
#9192=CARTESIAN_POINT('Ctrl Pts',(-1.57930034717566,-16.8195656763126,7.));
#9193=CARTESIAN_POINT('Ctrl Pts',(-1.57225556404312,-16.7804505865492,7.));
#9194=CARTESIAN_POINT('Ctrl Pts',(-1.56489594057218,-16.7455711436431,7.));
#9195=CARTESIAN_POINT('Ctrl Pts',(-1.55162638755018,-16.6896454316358,7.));
#9196=CARTESIAN_POINT('Ctrl Pts',(-1.52918899676863,-16.6138949491149,7.));
#9197=CARTESIAN_POINT('Ctrl Pts',(-1.49051796169811,-16.5198135565977,7.));
#9198=CARTESIAN_POINT('Ctrl Pts',(-1.43783746532133,-16.4279450992207,7.));
#9199=CARTESIAN_POINT('Ctrl Pts',(-1.3620126454106,-16.3372938385016,7.));
#9200=CARTESIAN_POINT('Ctrl Pts',(-1.23650382033378,-16.2452435266959,7.));
#9201=CARTESIAN_POINT('Ctrl Pts',(-1.1199417984865,-16.2167242606458,7.));
#9202=CARTESIAN_POINT('Ctrl Pts',(-1.04967429885986,-16.2160625265911,7.));
#9203=CARTESIAN_POINT('',(1.04967429885974,-16.2160625265911,7.));
#9204=CARTESIAN_POINT('Origin',(0.,0.,7.));
#9205=CARTESIAN_POINT('',(2.47738131311187,-18.8377966288376,7.));
#9206=CARTESIAN_POINT('Ctrl Pts',(1.04967429885974,-16.2160625265911,7.));
#9207=CARTESIAN_POINT('Ctrl Pts',(1.11994179848648,-16.2167242606459,7.));
#9208=CARTESIAN_POINT('Ctrl Pts',(1.23650382033375,-16.2452435266959,7.));
#9209=CARTESIAN_POINT('Ctrl Pts',(1.36201264541055,-16.3372938385016,7.));
#9210=CARTESIAN_POINT('Ctrl Pts',(1.4378374653213,-16.4279450992208,7.));
#9211=CARTESIAN_POINT('Ctrl Pts',(1.4905179616981,-16.5198135565978,7.));
#9212=CARTESIAN_POINT('Ctrl Pts',(1.52918899676862,-16.6138949491149,7.));
#9213=CARTESIAN_POINT('Ctrl Pts',(1.55162638755016,-16.6896454316359,7.));
#9214=CARTESIAN_POINT('Ctrl Pts',(1.56489594057218,-16.7455711436431,7.));
#9215=CARTESIAN_POINT('Ctrl Pts',(1.57225556404312,-16.7804505865492,7.));
#9216=CARTESIAN_POINT('Ctrl Pts',(1.57930034717562,-16.8195656763126,7.));
#9217=CARTESIAN_POINT('Ctrl Pts',(1.58971419725804,-16.8793055486399,7.));
#9218=CARTESIAN_POINT('Ctrl Pts',(1.60803840593144,-16.9659973771906,7.));
#9219=CARTESIAN_POINT('Ctrl Pts',(1.6370032466926,-17.0826338282622,7.));
#9220=CARTESIAN_POINT('Ctrl Pts',(1.67639424155263,-17.2191007779953,7.));
#9221=CARTESIAN_POINT('Ctrl Pts',(1.72763282051121,-17.3747717371572,7.));
#9222=CARTESIAN_POINT('Ctrl Pts',(1.79222730418269,-17.548917731071,7.));
#9223=CARTESIAN_POINT('Ctrl Pts',(1.87160676754277,-17.7407325407201,7.));
#9224=CARTESIAN_POINT('Ctrl Pts',(1.96717098182925,-17.949326772361,7.));
#9225=CARTESIAN_POINT('Ctrl Pts',(2.08026807216972,-18.1737325312257,7.));
#9226=CARTESIAN_POINT('Ctrl Pts',(2.2465324944921,-18.4751451900744,7.));
#9227=CARTESIAN_POINT('Ctrl Pts',(2.38389175781394,-18.6965496529788,7.));
#9228=CARTESIAN_POINT('Ctrl Pts',(2.47738131311187,-18.8377966288376,7.));
#9229=CARTESIAN_POINT('',(3.46506965370692,-18.6813621637974,7.));
#9230=CARTESIAN_POINT('Origin',(0.,0.,7.));
#9231=CARTESIAN_POINT('',(4.01273932064523,-15.7467591314704,7.));
#9232=CARTESIAN_POINT('Ctrl Pts',(3.46506965370692,-18.6813621637974,7.));
#9233=CARTESIAN_POINT('Ctrl Pts',(3.51033578853419,-18.5181384456162,7.));
#9234=CARTESIAN_POINT('Ctrl Pts',(3.57255446932203,-18.2651239417329,7.));
#9235=CARTESIAN_POINT('Ctrl Pts',(3.63753969769579,-17.9270849363835,7.));
#9236=CARTESIAN_POINT('Ctrl Pts',(3.67575622931334,-17.6787134541915,7.));
#9237=CARTESIAN_POINT('Ctrl Pts',(3.7021840355295,-17.4507975846592,7.));
#9238=CARTESIAN_POINT('Ctrl Pts',(3.71840435546372,-17.2438412568379,7.));
#9239=CARTESIAN_POINT('Ctrl Pts',(3.72602328845457,-17.0582577813421,7.));
#9240=CARTESIAN_POINT('Ctrl Pts',(3.72664910094712,-16.8943723095674,7.));
#9241=CARTESIAN_POINT('Ctrl Pts',(3.72194155665404,-16.7524120409277,7.));
#9242=CARTESIAN_POINT('Ctrl Pts',(3.71344611165872,-16.632533556064,7.));
#9243=CARTESIAN_POINT('Ctrl Pts',(3.70408422142791,-16.5444222357228,7.));
#9244=CARTESIAN_POINT('Ctrl Pts',(3.69552774561757,-16.4843881842109,7.));
#9245=CARTESIAN_POINT('Ctrl Pts',(3.69014050504827,-16.4450105654963,7.));
#9246=CARTESIAN_POINT('Ctrl Pts',(3.68636158229547,-16.409563995311,7.));
#9247=CARTESIAN_POINT('Ctrl Pts',(3.68169968173261,-16.3522749650865,7.));
#9248=CARTESIAN_POINT('Ctrl Pts',(3.67963072201297,-16.2732984400115,7.));
#9249=CARTESIAN_POINT('Ctrl Pts',(3.68733631276642,-16.1718717115691,7.));
#9250=CARTESIAN_POINT('Ctrl Pts',(3.70904952755071,-16.0682204478862,7.));
#9251=CARTESIAN_POINT('Ctrl Pts',(3.75315043649999,-15.958574817721,7.));
#9252=CARTESIAN_POINT('Ctrl Pts',(3.84407131175639,-15.8322454089585,7.));
#9253=CARTESIAN_POINT('Ctrl Pts',(3.94611544431021,-15.7691023294921,7.));
#9254=CARTESIAN_POINT('Ctrl Pts',(4.01273932064523,-15.7467591314704,7.));
#9255=CARTESIAN_POINT('',(6.00933848448151,-15.0980247376579,7.));
#9256=CARTESIAN_POINT('Origin',(0.,0.,7.));
#9257=CARTESIAN_POINT('',(8.17732893607279,-17.1502563092004,7.));
#9258=CARTESIAN_POINT('Ctrl Pts',(6.00933848448151,-15.0980247376579,7.));
#9259=CARTESIAN_POINT('Ctrl Pts',(6.07637133495396,-15.0769402326058,7.));
#9260=CARTESIAN_POINT('Ctrl Pts',(6.1960413432609,-15.0680440207731,7.));
#9261=CARTESIAN_POINT('Ctrl Pts',(6.34385243988821,-15.1168047097502,7.));
#9262=CARTESIAN_POINT('Ctrl Pts',(6.44397890908497,-15.1795880240196,7.));
#9263=CARTESIAN_POINT('Ctrl Pts',(6.52246995302229,-15.2506809503975,7.));
#9264=CARTESIAN_POINT('Ctrl Pts',(6.58832104206024,-15.3282076647862,7.));
#9265=CARTESIAN_POINT('Ctrl Pts',(6.63306845520277,-15.3933171197393,7.));
#9266=CARTESIAN_POINT('Ctrl Pts',(6.66297054550544,-15.4424051151807,7.));
#9267=CARTESIAN_POINT('Ctrl Pts',(6.68074830397727,-15.4733031879166,7.));
#9268=CARTESIAN_POINT('Ctrl Pts',(6.69953551835471,-15.5083268912119,7.));
#9269=CARTESIAN_POINT('Ctrl Pts',(6.72790031412625,-15.5619248294191,7.));
#9270=CARTESIAN_POINT('Ctrl Pts',(6.77211692048664,-15.6387111659832,7.));
#9271=CARTESIAN_POINT('Ctrl Pts',(6.83570676658069,-15.7406883947778,7.));
#9272=CARTESIAN_POINT('Ctrl Pts',(6.91534043556371,-15.8583036897433,7.));
#9273=CARTESIAN_POINT('Ctrl Pts',(7.01217619187964,-15.9905219781863,7.));
#9274=CARTESIAN_POINT('Ctrl Pts',(7.12742326811382,-16.1361838672874,7.));
#9275=CARTESIAN_POINT('Ctrl Pts',(7.2621916599568,-16.2940809887434,7.));
#9276=CARTESIAN_POINT('Ctrl Pts',(7.41753779118422,-16.4629349257385,7.));
#9277=CARTESIAN_POINT('Ctrl Pts',(7.59444470905135,-16.6414085620714,7.));
#9278=CARTESIAN_POINT('Ctrl Pts',(7.84571320523309,-16.8766905033058,7.));
#9279=CARTESIAN_POINT('Ctrl Pts',(8.04476736935673,-17.0448123137865,7.));
#9280=CARTESIAN_POINT('Ctrl Pts',(8.17732893607279,-17.1502563092004,7.));
#9281=CARTESIAN_POINT('',(9.06833546026109,-16.6962658094609,7.));
#9282=CARTESIAN_POINT('Origin',(0.,0.,7.));
#9283=CARTESIAN_POINT('',(8.68235805704667,-13.7360532384392,7.));
#9284=CARTESIAN_POINT('Ctrl Pts',(9.06833546026109,-16.6962658094609,7.));
#9285=CARTESIAN_POINT('Ctrl Pts',(9.06094720995301,-16.5270428237395,7.));
#9286=CARTESIAN_POINT('Ctrl Pts',(9.0419349102283,-16.267185101373,7.));
#9287=CARTESIAN_POINT('Ctrl Pts',(8.99927973772149,-15.9256093626227,7.));
#9288=CARTESIAN_POINT('Ctrl Pts',(8.95887481023114,-15.6775844882862,7.));
#9289=CARTESIAN_POINT('Ctrl Pts',(8.91357927057119,-15.4526569741556,7.));
#9290=CARTESIAN_POINT('Ctrl Pts',(8.8650526891508,-15.2508174554787,7.));
#9291=CARTESIAN_POINT('Ctrl Pts',(8.81495027721559,-15.0719627020186,7.));
#9292=CARTESIAN_POINT('Ctrl Pts',(8.76490206435508,-14.9159049694657,7.));
#9293=CARTESIAN_POINT('Ctrl Pts',(8.7165567881437,-14.7823474421092,7.));
#9294=CARTESIAN_POINT('Ctrl Pts',(8.67143265073927,-14.6709614647944,7.));
#9295=CARTESIAN_POINT('Ctrl Pts',(8.63530106864817,-14.5900556026053,7.));
#9296=CARTESIAN_POINT('Ctrl Pts',(8.60861183441386,-14.5356039231526,7.));
#9297=CARTESIAN_POINT('Ctrl Pts',(8.59131991078477,-14.4998183311667,7.));
#9298=CARTESIAN_POINT('Ctrl Pts',(8.57677234909656,-14.4672743909626,7.));
#9299=CARTESIAN_POINT('Ctrl Pts',(8.55463533425731,-14.4142298919554,7.));
#9300=CARTESIAN_POINT('Ctrl Pts',(8.52826254822914,-14.3397580968625,7.));
#9301=CARTESIAN_POINT('Ctrl Pts',(8.50424841775455,-14.2409143873564,7.));
#9302=CARTESIAN_POINT('Ctrl Pts',(8.49286891019841,-14.1356264252376,7.));
#9303=CARTESIAN_POINT('Ctrl Pts',(8.50092900394917,-14.0177193038531,7.));
#9304=CARTESIAN_POINT('Ctrl Pts',(8.54836196063206,-13.8694768008521,7.));
#9305=CARTESIAN_POINT('Ctrl Pts',(8.62589941321478,-13.7778907925312,7.));
#9306=CARTESIAN_POINT('Ctrl Pts',(8.68235805704667,-13.7360532384392,7.));
#9307=CARTESIAN_POINT('',(10.3807667497191,-12.5020870932787,7.));
#9308=CARTESIAN_POINT('Origin',(0.,0.,7.));
#9309=CARTESIAN_POINT('',(13.07682262797,-13.7839294091566,7.));
#9310=CARTESIAN_POINT('Ctrl Pts',(10.3807667497191,-12.5020870932787,7.));
#9311=CARTESIAN_POINT('Ctrl Pts',(10.4380033085876,-12.4613202473788,7.));
#9312=CARTESIAN_POINT('Ctrl Pts',(10.5490671691512,-12.4158793808611,7.));
#9313=CARTESIAN_POINT('Ctrl Pts',(10.7047117573306,-12.4165774110367,7.));
#9314=CARTESIAN_POINT('Ctrl Pts',(10.8193387993863,-12.4453471106188,7.));
#9315=CARTESIAN_POINT('Ctrl Pts',(10.9159571406243,-12.48870543503,7.));
#9316=CARTESIAN_POINT('Ctrl Pts',(11.0025423202231,-12.5420886163255,7.));
#9317=CARTESIAN_POINT('Ctrl Pts',(11.0652195671547,-12.5901836766158,7.));
#9318=CARTESIAN_POINT('Ctrl Pts',(11.1088271697991,-12.6276288804813,7.));
#9319=CARTESIAN_POINT('Ctrl Pts',(11.1352828524077,-12.651521064408,7.));
#9320=CARTESIAN_POINT('Ctrl Pts',(11.1639734745885,-12.6790250171322,7.));
#9321=CARTESIAN_POINT('Ctrl Pts',(11.2075126722099,-12.7212344815888,7.));
#9322=CARTESIAN_POINT('Ctrl Pts',(11.2732934467515,-12.7805989445416,7.));
#9323=CARTESIAN_POINT('Ctrl Pts',(11.3652836809863,-12.8579347093876,7.));
#9324=CARTESIAN_POINT('Ctrl Pts',(11.4773649257318,-12.9451853450404,7.));
#9325=CARTESIAN_POINT('Ctrl Pts',(11.6103189008825,-13.0410085154727,7.));
#9326=CARTESIAN_POINT('Ctrl Pts',(11.764937382884,-13.1439278991698,7.));
#9327=CARTESIAN_POINT('Ctrl Pts',(11.9419026340297,-13.2524512620507,7.));
#9328=CARTESIAN_POINT('Ctrl Pts',(12.1418243205134,-13.3650363045724,7.));
#9329=CARTESIAN_POINT('Ctrl Pts',(12.3652241842034,-13.4801075753502,7.));
#9330=CARTESIAN_POINT('Ctrl Pts',(12.6769008431476,-13.6262277632565,7.));
#9331=CARTESIAN_POINT('Ctrl Pts',(12.9181650995967,-13.7246099871303,7.));
#9332=CARTESIAN_POINT('Ctrl Pts',(13.07682262797,-13.7839294091566,7.));
#9333=CARTESIAN_POINT('',(13.7839294091565,-13.0768226279701,7.));
#9334=CARTESIAN_POINT('Origin',(0.,1.10390771809154E-15,7.));
#9335=CARTESIAN_POINT('',(12.5020870932787,-10.3807667497191,7.));
#9336=CARTESIAN_POINT('Ctrl Pts',(13.7839294091565,-13.0768226279701,7.));
#9337=CARTESIAN_POINT('Ctrl Pts',(13.7246099871302,-12.9181650995967,7.));
#9338=CARTESIAN_POINT('Ctrl Pts',(13.6262277632565,-12.6769008431476,7.));
#9339=CARTESIAN_POINT('Ctrl Pts',(13.4801075753502,-12.3652241842034,7.));
#9340=CARTESIAN_POINT('Ctrl Pts',(13.3650363045723,-12.1418243205134,7.));
#9341=CARTESIAN_POINT('Ctrl Pts',(13.2524512620508,-11.9419026340297,7.));
#9342=CARTESIAN_POINT('Ctrl Pts',(13.1439278991698,-11.764937382884,7.));
#9343=CARTESIAN_POINT('Ctrl Pts',(13.0410085154728,-11.6103189008825,7.));
#9344=CARTESIAN_POINT('Ctrl Pts',(12.9451853450404,-11.4773649257318,7.));
#9345=CARTESIAN_POINT('Ctrl Pts',(12.8579347093876,-11.3652836809863,7.));
#9346=CARTESIAN_POINT('Ctrl Pts',(12.7805989445416,-11.2732934467515,7.));
#9347=CARTESIAN_POINT('Ctrl Pts',(12.7212344815888,-11.2075126722099,7.));
#9348=CARTESIAN_POINT('Ctrl Pts',(12.6790250171322,-11.1639734745885,7.));
#9349=CARTESIAN_POINT('Ctrl Pts',(12.6515210644081,-11.1352828524076,7.));
#9350=CARTESIAN_POINT('Ctrl Pts',(12.6276288804813,-11.108827169799,7.));
#9351=CARTESIAN_POINT('Ctrl Pts',(12.5901836766158,-11.0652195671547,7.));
#9352=CARTESIAN_POINT('Ctrl Pts',(12.5420886163255,-11.0025423202231,7.));
#9353=CARTESIAN_POINT('Ctrl Pts',(12.48870543503,-10.9159571406243,7.));
#9354=CARTESIAN_POINT('Ctrl Pts',(12.4453471106188,-10.8193387993863,7.));
#9355=CARTESIAN_POINT('Ctrl Pts',(12.4165774110367,-10.7047117573306,7.));
#9356=CARTESIAN_POINT('Ctrl Pts',(12.4158793808611,-10.5490671691512,7.));
#9357=CARTESIAN_POINT('Ctrl Pts',(12.4613202473788,-10.4380033085876,7.));
#9358=CARTESIAN_POINT('Ctrl Pts',(12.5020870932787,-10.3807667497191,7.));
#9359=CARTESIAN_POINT('',(13.7360532384392,-8.68235805704669,7.));
#9360=CARTESIAN_POINT('Origin',(0.,0.,7.));
#9361=CARTESIAN_POINT('',(16.6962658094608,-9.06833546026116,7.));
#9362=CARTESIAN_POINT('Ctrl Pts',(13.7360532384392,-8.68235805704669,7.));
#9363=CARTESIAN_POINT('Ctrl Pts',(13.7778907925313,-8.62589941321482,7.));
#9364=CARTESIAN_POINT('Ctrl Pts',(13.8694768008521,-8.54836196063209,7.));
#9365=CARTESIAN_POINT('Ctrl Pts',(14.0177193038531,-8.50092900394922,7.));
#9366=CARTESIAN_POINT('Ctrl Pts',(14.1356264252377,-8.49286891019844,7.));
#9367=CARTESIAN_POINT('Ctrl Pts',(14.2409143873564,-8.50424841775457,7.));
#9368=CARTESIAN_POINT('Ctrl Pts',(14.3397580968626,-8.52826254822916,7.));
#9369=CARTESIAN_POINT('Ctrl Pts',(14.4142298919554,-8.55463533425733,7.));
#9370=CARTESIAN_POINT('Ctrl Pts',(14.4672743909627,-8.57677234909657,7.));
#9371=CARTESIAN_POINT('Ctrl Pts',(14.4998183311667,-8.59131991078477,7.));
#9372=CARTESIAN_POINT('Ctrl Pts',(14.5356039231527,-8.6086118344139,7.));
#9373=CARTESIAN_POINT('Ctrl Pts',(14.5900556026053,-8.63530106864818,7.));
#9374=CARTESIAN_POINT('Ctrl Pts',(14.6709614647944,-8.67143265073928,7.));
#9375=CARTESIAN_POINT('Ctrl Pts',(14.7823474421092,-8.71655678814373,7.));
#9376=CARTESIAN_POINT('Ctrl Pts',(14.9159049694657,-8.7649020643551,7.));
#9377=CARTESIAN_POINT('Ctrl Pts',(15.0719627020186,-8.81495027721557,7.));
#9378=CARTESIAN_POINT('Ctrl Pts',(15.2508174554788,-8.86505268915084,7.));
#9379=CARTESIAN_POINT('Ctrl Pts',(15.4526569741556,-8.91357927057117,7.));
#9380=CARTESIAN_POINT('Ctrl Pts',(15.6775844882862,-8.95887481023116,7.));
#9381=CARTESIAN_POINT('Ctrl Pts',(15.9256093626227,-8.99927973772153,7.));
#9382=CARTESIAN_POINT('Ctrl Pts',(16.2671851013731,-9.04193491022831,7.));
#9383=CARTESIAN_POINT('Ctrl Pts',(16.5270428237395,-9.06094720995305,7.));
#9384=CARTESIAN_POINT('Ctrl Pts',(16.6962658094608,-9.06833546026116,7.));
#9385=CARTESIAN_POINT('',(17.1502563092003,-8.17732893607285,7.));
#9386=CARTESIAN_POINT('Origin',(0.,0.,7.));
#9387=CARTESIAN_POINT('',(15.0980247376579,-6.00933848448159,7.));
#9388=CARTESIAN_POINT('Ctrl Pts',(17.1502563092003,-8.17732893607285,7.));
#9389=CARTESIAN_POINT('Ctrl Pts',(17.0448123137865,-8.04476736935674,7.));
#9390=CARTESIAN_POINT('Ctrl Pts',(16.8766905033057,-7.84571320523309,7.));
#9391=CARTESIAN_POINT('Ctrl Pts',(16.6414085620714,-7.59444470905136,7.));
#9392=CARTESIAN_POINT('Ctrl Pts',(16.4629349257385,-7.41753779118421,7.));
#9393=CARTESIAN_POINT('Ctrl Pts',(16.2940809887434,-7.26219165995679,7.));
#9394=CARTESIAN_POINT('Ctrl Pts',(16.1361838672874,-7.12742326811383,7.));
#9395=CARTESIAN_POINT('Ctrl Pts',(15.9905219781863,-7.01217619187962,7.));
#9396=CARTESIAN_POINT('Ctrl Pts',(15.8583036897433,-6.91534043556369,7.));
#9397=CARTESIAN_POINT('Ctrl Pts',(15.7406883947777,-6.83570676658069,7.));
#9398=CARTESIAN_POINT('Ctrl Pts',(15.6387111659832,-6.77211692048663,7.));
#9399=CARTESIAN_POINT('Ctrl Pts',(15.5619248294191,-6.72790031412624,7.));
#9400=CARTESIAN_POINT('Ctrl Pts',(15.5083268912119,-6.69953551835472,7.));
#9401=CARTESIAN_POINT('Ctrl Pts',(15.4733031879166,-6.68074830397725,7.));
#9402=CARTESIAN_POINT('Ctrl Pts',(15.4424051151807,-6.66297054550541,7.));
#9403=CARTESIAN_POINT('Ctrl Pts',(15.3933171197393,-6.63306845520276,7.));
#9404=CARTESIAN_POINT('Ctrl Pts',(15.3282076647862,-6.58832104206022,7.));
#9405=CARTESIAN_POINT('Ctrl Pts',(15.2506809503975,-6.52246995302226,7.));
#9406=CARTESIAN_POINT('Ctrl Pts',(15.1795880240196,-6.44397890908496,7.));
#9407=CARTESIAN_POINT('Ctrl Pts',(15.1168047097501,-6.34385243988822,7.));
#9408=CARTESIAN_POINT('Ctrl Pts',(15.0680440207731,-6.1960413432609,7.));
#9409=CARTESIAN_POINT('Ctrl Pts',(15.0769402326058,-6.07637133495394,7.));
#9410=CARTESIAN_POINT('Ctrl Pts',(15.0980247376579,-6.00933848448159,7.));
#9411=CARTESIAN_POINT('',(15.7467591314704,-4.01273932064523,7.));
#9412=CARTESIAN_POINT('Origin',(0.,0.,7.));
#9413=CARTESIAN_POINT('',(18.6813621637973,-3.46506965370701,7.));
#9414=CARTESIAN_POINT('Ctrl Pts',(15.7467591314704,-4.01273932064523,7.));
#9415=CARTESIAN_POINT('Ctrl Pts',(15.7691023294921,-3.94611544431022,7.));
#9416=CARTESIAN_POINT('Ctrl Pts',(15.8322454089585,-3.8440713117564,7.));
#9417=CARTESIAN_POINT('Ctrl Pts',(15.958574817721,-3.75315043650002,7.));
#9418=CARTESIAN_POINT('Ctrl Pts',(16.0682204478862,-3.70904952755073,7.));
#9419=CARTESIAN_POINT('Ctrl Pts',(16.1718717115691,-3.68733631276642,7.));
#9420=CARTESIAN_POINT('Ctrl Pts',(16.2732984400115,-3.67963072201298,7.));
#9421=CARTESIAN_POINT('Ctrl Pts',(16.3522749650865,-3.68169968173262,7.));
#9422=CARTESIAN_POINT('Ctrl Pts',(16.409563995311,-3.68636158229546,7.));
#9423=CARTESIAN_POINT('Ctrl Pts',(16.4450105654963,-3.69014050504826,7.));
#9424=CARTESIAN_POINT('Ctrl Pts',(16.4843881842109,-3.6955277456176,7.));
#9425=CARTESIAN_POINT('Ctrl Pts',(16.5444222357228,-3.70408422142792,7.));
#9426=CARTESIAN_POINT('Ctrl Pts',(16.632533556064,-3.71344611165872,7.));
#9427=CARTESIAN_POINT('Ctrl Pts',(16.7524120409277,-3.72194155665406,7.));
#9428=CARTESIAN_POINT('Ctrl Pts',(16.8943723095674,-3.72664910094713,7.));
#9429=CARTESIAN_POINT('Ctrl Pts',(17.0582577813421,-3.72602328845455,7.));
#9430=CARTESIAN_POINT('Ctrl Pts',(17.2438412568379,-3.71840435546376,7.));
#9431=CARTESIAN_POINT('Ctrl Pts',(17.4507975846592,-3.70218403552949,7.));
#9432=CARTESIAN_POINT('Ctrl Pts',(17.6787134541915,-3.67575622931335,7.));
#9433=CARTESIAN_POINT('Ctrl Pts',(17.9270849363835,-3.63753969769582,7.));
#9434=CARTESIAN_POINT('Ctrl Pts',(18.265123941733,-3.57255446932205,7.));
#9435=CARTESIAN_POINT('Ctrl Pts',(18.5181384456163,-3.51033578853422,7.));
#9436=CARTESIAN_POINT('Ctrl Pts',(18.6813621637973,-3.46506965370701,7.));
#9437=CARTESIAN_POINT('',(18.8377966288376,-2.47738131311191,7.));
#9438=CARTESIAN_POINT('Origin',(0.,0.,7.));
#9439=CARTESIAN_POINT('',(16.2160625265911,-1.04967429885982,7.));
#9440=CARTESIAN_POINT('Ctrl Pts',(18.8377966288376,-2.47738131311191,7.));
#9441=CARTESIAN_POINT('Ctrl Pts',(18.6965496529788,-2.38389175781396,7.));
#9442=CARTESIAN_POINT('Ctrl Pts',(18.4751451900744,-2.24653249449211,7.));
#9443=CARTESIAN_POINT('Ctrl Pts',(18.1737325312257,-2.08026807216974,7.));
#9444=CARTESIAN_POINT('Ctrl Pts',(17.949326772361,-1.96717098182924,7.));
#9445=CARTESIAN_POINT('Ctrl Pts',(17.7407325407201,-1.87160676754275,7.));
#9446=CARTESIAN_POINT('Ctrl Pts',(17.548917731071,-1.7922273041827,7.));
#9447=CARTESIAN_POINT('Ctrl Pts',(17.3747717371572,-1.72763282051117,7.));
#9448=CARTESIAN_POINT('Ctrl Pts',(17.2191007779952,-1.67639424155261,7.));
#9449=CARTESIAN_POINT('Ctrl Pts',(17.0826338282621,-1.6370032466926,7.));
#9450=CARTESIAN_POINT('Ctrl Pts',(16.9659973771906,-1.60803840593143,7.));
#9451=CARTESIAN_POINT('Ctrl Pts',(16.8793055486399,-1.58971419725802,7.));
#9452=CARTESIAN_POINT('Ctrl Pts',(16.8195656763126,-1.57930034717563,7.));
#9453=CARTESIAN_POINT('Ctrl Pts',(16.7804505865492,-1.57225556404309,7.));
#9454=CARTESIAN_POINT('Ctrl Pts',(16.7455711436431,-1.56489594057215,7.));
#9455=CARTESIAN_POINT('Ctrl Pts',(16.6896454316358,-1.55162638755015,7.));
#9456=CARTESIAN_POINT('Ctrl Pts',(16.6138949491149,-1.5291889967686,7.));
#9457=CARTESIAN_POINT('Ctrl Pts',(16.5198135565977,-1.49051796169807,7.));
#9458=CARTESIAN_POINT('Ctrl Pts',(16.4279450992207,-1.43783746532129,7.));
#9459=CARTESIAN_POINT('Ctrl Pts',(16.3372938385016,-1.36201264541057,7.));
#9460=CARTESIAN_POINT('Ctrl Pts',(16.2452435266959,-1.23650382033374,7.));
#9461=CARTESIAN_POINT('Ctrl Pts',(16.2167242606458,-1.11994179848647,7.));
#9462=CARTESIAN_POINT('Ctrl Pts',(16.2160625265911,-1.04967429885982,7.));
#9463=CARTESIAN_POINT('',(16.2160625265911,1.0496742988598,7.));
#9464=CARTESIAN_POINT('Origin',(0.,0.,7.));
#9465=CARTESIAN_POINT('',(18.8377966288376,2.47738131311188,7.));
#9466=CARTESIAN_POINT('Ctrl Pts',(16.2160625265911,1.0496742988598,7.));
#9467=CARTESIAN_POINT('Ctrl Pts',(16.2167242606459,1.11994179848647,7.));
#9468=CARTESIAN_POINT('Ctrl Pts',(16.2452435266959,1.23650382033374,7.));
#9469=CARTESIAN_POINT('Ctrl Pts',(16.3372938385016,1.36201264541054,7.));
#9470=CARTESIAN_POINT('Ctrl Pts',(16.4279450992208,1.43783746532129,7.));
#9471=CARTESIAN_POINT('Ctrl Pts',(16.5198135565978,1.49051796169809,7.));
#9472=CARTESIAN_POINT('Ctrl Pts',(16.6138949491149,1.52918899676861,7.));
#9473=CARTESIAN_POINT('Ctrl Pts',(16.6896454316359,1.55162638755015,7.));
#9474=CARTESIAN_POINT('Ctrl Pts',(16.7455711436431,1.56489594057217,7.));
#9475=CARTESIAN_POINT('Ctrl Pts',(16.7804505865492,1.57225556404311,7.));
#9476=CARTESIAN_POINT('Ctrl Pts',(16.8195656763126,1.57930034717561,7.));
#9477=CARTESIAN_POINT('Ctrl Pts',(16.8793055486399,1.58971419725803,7.));
#9478=CARTESIAN_POINT('Ctrl Pts',(16.9659973771906,1.60803840593143,7.));
#9479=CARTESIAN_POINT('Ctrl Pts',(17.0826338282621,1.63700324669259,7.));
#9480=CARTESIAN_POINT('Ctrl Pts',(17.2191007779953,1.67639424155262,7.));
#9481=CARTESIAN_POINT('Ctrl Pts',(17.3747717371572,1.7276328205112,7.));
#9482=CARTESIAN_POINT('Ctrl Pts',(17.548917731071,1.79222730418268,7.));
#9483=CARTESIAN_POINT('Ctrl Pts',(17.7407325407201,1.87160676754277,7.));
#9484=CARTESIAN_POINT('Ctrl Pts',(17.949326772361,1.96717098182924,7.));
#9485=CARTESIAN_POINT('Ctrl Pts',(18.1737325312257,2.08026807216972,7.));
#9486=CARTESIAN_POINT('Ctrl Pts',(18.4751451900744,2.2465324944921,7.));
#9487=CARTESIAN_POINT('Ctrl Pts',(18.6965496529788,2.38389175781394,7.));
#9488=CARTESIAN_POINT('Ctrl Pts',(18.8377966288376,2.47738131311188,7.));
#9489=CARTESIAN_POINT('',(18.6813621637973,3.46506965370699,7.));
#9490=CARTESIAN_POINT('Origin',(1.73472347597681E-15,0.,7.));
#9491=CARTESIAN_POINT('',(15.7467591314704,4.01273932064524,7.));
#9492=CARTESIAN_POINT('Ctrl Pts',(18.6813621637973,3.46506965370699,7.));
#9493=CARTESIAN_POINT('Ctrl Pts',(18.5181384456162,3.51033578853419,7.));
#9494=CARTESIAN_POINT('Ctrl Pts',(18.2651239417329,3.57255446932204,7.));
#9495=CARTESIAN_POINT('Ctrl Pts',(17.9270849363835,3.63753969769579,7.));
#9496=CARTESIAN_POINT('Ctrl Pts',(17.6787134541915,3.67575622931334,7.));
#9497=CARTESIAN_POINT('Ctrl Pts',(17.4507975846592,3.70218403552951,7.));
#9498=CARTESIAN_POINT('Ctrl Pts',(17.2438412568379,3.71840435546372,7.));
#9499=CARTESIAN_POINT('Ctrl Pts',(17.0582577813421,3.72602328845457,7.));
#9500=CARTESIAN_POINT('Ctrl Pts',(16.8943723095674,3.72664910094712,7.));
#9501=CARTESIAN_POINT('Ctrl Pts',(16.7524120409277,3.72194155665404,7.));
#9502=CARTESIAN_POINT('Ctrl Pts',(16.632533556064,3.71344611165872,7.));
#9503=CARTESIAN_POINT('Ctrl Pts',(16.5444222357228,3.70408422142792,7.));
#9504=CARTESIAN_POINT('Ctrl Pts',(16.4843881842109,3.69552774561757,7.));
#9505=CARTESIAN_POINT('Ctrl Pts',(16.4450105654963,3.69014050504827,7.));
#9506=CARTESIAN_POINT('Ctrl Pts',(16.409563995311,3.68636158229547,7.));
#9507=CARTESIAN_POINT('Ctrl Pts',(16.3522749650865,3.68169968173261,7.));
#9508=CARTESIAN_POINT('Ctrl Pts',(16.2732984400115,3.67963072201297,7.));
#9509=CARTESIAN_POINT('Ctrl Pts',(16.1718717115691,3.68733631276642,7.));
#9510=CARTESIAN_POINT('Ctrl Pts',(16.0682204478862,3.70904952755071,7.));
#9511=CARTESIAN_POINT('Ctrl Pts',(15.958574817721,3.75315043649999,7.));
#9512=CARTESIAN_POINT('Ctrl Pts',(15.8322454089585,3.84407131175639,7.));
#9513=CARTESIAN_POINT('Ctrl Pts',(15.7691023294921,3.94611544431022,7.));
#9514=CARTESIAN_POINT('Ctrl Pts',(15.7467591314704,4.01273932064524,7.));
#9515=CARTESIAN_POINT('Origin',(0.,0.,7.));
#9516=CARTESIAN_POINT('Origin',(16.0675296603332,7.07348467874013,0.));
#9517=CARTESIAN_POINT('',(15.0980247376579,6.00933848448158,0.));
#9518=CARTESIAN_POINT('',(17.1502563092004,8.17732893607278,0.));
#9519=CARTESIAN_POINT('Ctrl Pts',(15.0980247376579,6.00933848448158,0.));
#9520=CARTESIAN_POINT('Ctrl Pts',(15.0769402326058,6.07637133495396,0.));
#9521=CARTESIAN_POINT('Ctrl Pts',(15.0680440207731,6.1960413432609,0.));
#9522=CARTESIAN_POINT('Ctrl Pts',(15.1168047097502,6.34385243988821,0.));
#9523=CARTESIAN_POINT('Ctrl Pts',(15.1795880240196,6.44397890908497,0.));
#9524=CARTESIAN_POINT('Ctrl Pts',(15.2506809503975,6.52246995302229,0.));
#9525=CARTESIAN_POINT('Ctrl Pts',(15.3282076647862,6.58832104206024,0.));
#9526=CARTESIAN_POINT('Ctrl Pts',(15.3933171197393,6.63306845520277,0.));
#9527=CARTESIAN_POINT('Ctrl Pts',(15.4424051151807,6.66297054550544,0.));
#9528=CARTESIAN_POINT('Ctrl Pts',(15.4733031879166,6.68074830397728,0.));
#9529=CARTESIAN_POINT('Ctrl Pts',(15.5083268912119,6.69953551835471,0.));
#9530=CARTESIAN_POINT('Ctrl Pts',(15.5619248294191,6.72790031412625,0.));
#9531=CARTESIAN_POINT('Ctrl Pts',(15.6387111659832,6.77211692048664,0.));
#9532=CARTESIAN_POINT('Ctrl Pts',(15.7406883947778,6.83570676658069,0.));
#9533=CARTESIAN_POINT('Ctrl Pts',(15.8583036897433,6.91534043556371,0.));
#9534=CARTESIAN_POINT('Ctrl Pts',(15.9905219781863,7.01217619187965,0.));
#9535=CARTESIAN_POINT('Ctrl Pts',(16.1361838672874,7.12742326811382,0.));
#9536=CARTESIAN_POINT('Ctrl Pts',(16.2940809887434,7.2621916599568,0.));
#9537=CARTESIAN_POINT('Ctrl Pts',(16.4629349257385,7.41753779118422,0.));
#9538=CARTESIAN_POINT('Ctrl Pts',(16.6414085620714,7.59444470905136,0.));
#9539=CARTESIAN_POINT('Ctrl Pts',(16.8766905033057,7.84571320523309,0.));
#9540=CARTESIAN_POINT('Ctrl Pts',(17.0448123137865,8.04476736935674,0.));
#9541=CARTESIAN_POINT('Ctrl Pts',(17.1502563092004,8.17732893607278,0.));
#9542=CARTESIAN_POINT('',(15.7467591314704,4.01273932064524,0.));
#9543=CARTESIAN_POINT('Origin',(0.,0.,0.));
#9544=CARTESIAN_POINT('',(18.6813621637973,3.46506965370699,0.));
#9545=CARTESIAN_POINT('Ctrl Pts',(18.6813621637973,3.46506965370699,0.));
#9546=CARTESIAN_POINT('Ctrl Pts',(18.5181384456162,3.51033578853419,0.));
#9547=CARTESIAN_POINT('Ctrl Pts',(18.2651239417329,3.57255446932204,0.));
#9548=CARTESIAN_POINT('Ctrl Pts',(17.9270849363835,3.63753969769579,0.));
#9549=CARTESIAN_POINT('Ctrl Pts',(17.6787134541915,3.67575622931334,0.));
#9550=CARTESIAN_POINT('Ctrl Pts',(17.4507975846592,3.70218403552951,0.));
#9551=CARTESIAN_POINT('Ctrl Pts',(17.2438412568379,3.71840435546372,0.));
#9552=CARTESIAN_POINT('Ctrl Pts',(17.0582577813421,3.72602328845457,0.));
#9553=CARTESIAN_POINT('Ctrl Pts',(16.8943723095674,3.72664910094712,0.));
#9554=CARTESIAN_POINT('Ctrl Pts',(16.7524120409277,3.72194155665404,0.));
#9555=CARTESIAN_POINT('Ctrl Pts',(16.632533556064,3.71344611165872,0.));
#9556=CARTESIAN_POINT('Ctrl Pts',(16.5444222357228,3.70408422142792,0.));
#9557=CARTESIAN_POINT('Ctrl Pts',(16.4843881842109,3.69552774561757,0.));
#9558=CARTESIAN_POINT('Ctrl Pts',(16.4450105654963,3.69014050504827,0.));
#9559=CARTESIAN_POINT('Ctrl Pts',(16.409563995311,3.68636158229547,0.));
#9560=CARTESIAN_POINT('Ctrl Pts',(16.3522749650865,3.68169968173261,0.));
#9561=CARTESIAN_POINT('Ctrl Pts',(16.2732984400115,3.67963072201297,0.));
#9562=CARTESIAN_POINT('Ctrl Pts',(16.1718717115691,3.68733631276642,0.));
#9563=CARTESIAN_POINT('Ctrl Pts',(16.0682204478862,3.70904952755071,0.));
#9564=CARTESIAN_POINT('Ctrl Pts',(15.958574817721,3.75315043649999,0.));
#9565=CARTESIAN_POINT('Ctrl Pts',(15.8322454089585,3.84407131175639,0.));
#9566=CARTESIAN_POINT('Ctrl Pts',(15.7691023294921,3.94611544431022,0.));
#9567=CARTESIAN_POINT('Ctrl Pts',(15.7467591314704,4.01273932064524,0.));
#9568=CARTESIAN_POINT('',(18.8377966288376,2.47738131311188,0.));
#9569=CARTESIAN_POINT('Origin',(1.73472347597681E-15,0.,0.));
#9570=CARTESIAN_POINT('',(16.2160625265911,1.0496742988598,0.));
#9571=CARTESIAN_POINT('Ctrl Pts',(16.2160625265911,1.0496742988598,0.));
#9572=CARTESIAN_POINT('Ctrl Pts',(16.2167242606459,1.11994179848647,0.));
#9573=CARTESIAN_POINT('Ctrl Pts',(16.2452435266959,1.23650382033374,0.));
#9574=CARTESIAN_POINT('Ctrl Pts',(16.3372938385016,1.36201264541054,0.));
#9575=CARTESIAN_POINT('Ctrl Pts',(16.4279450992208,1.43783746532129,0.));
#9576=CARTESIAN_POINT('Ctrl Pts',(16.5198135565978,1.49051796169809,0.));
#9577=CARTESIAN_POINT('Ctrl Pts',(16.6138949491149,1.52918899676861,0.));
#9578=CARTESIAN_POINT('Ctrl Pts',(16.6896454316359,1.55162638755015,0.));
#9579=CARTESIAN_POINT('Ctrl Pts',(16.7455711436431,1.56489594057217,0.));
#9580=CARTESIAN_POINT('Ctrl Pts',(16.7804505865492,1.57225556404311,0.));
#9581=CARTESIAN_POINT('Ctrl Pts',(16.8195656763126,1.57930034717561,0.));
#9582=CARTESIAN_POINT('Ctrl Pts',(16.8793055486399,1.58971419725803,0.));
#9583=CARTESIAN_POINT('Ctrl Pts',(16.9659973771906,1.60803840593143,0.));
#9584=CARTESIAN_POINT('Ctrl Pts',(17.0826338282621,1.63700324669259,0.));
#9585=CARTESIAN_POINT('Ctrl Pts',(17.2191007779953,1.67639424155262,0.));
#9586=CARTESIAN_POINT('Ctrl Pts',(17.3747717371572,1.7276328205112,0.));
#9587=CARTESIAN_POINT('Ctrl Pts',(17.548917731071,1.79222730418268,0.));
#9588=CARTESIAN_POINT('Ctrl Pts',(17.7407325407201,1.87160676754277,0.));
#9589=CARTESIAN_POINT('Ctrl Pts',(17.949326772361,1.96717098182924,0.));
#9590=CARTESIAN_POINT('Ctrl Pts',(18.1737325312257,2.08026807216972,0.));
#9591=CARTESIAN_POINT('Ctrl Pts',(18.4751451900744,2.2465324944921,0.));
#9592=CARTESIAN_POINT('Ctrl Pts',(18.6965496529788,2.38389175781394,0.));
#9593=CARTESIAN_POINT('Ctrl Pts',(18.8377966288376,2.47738131311188,0.));
#9594=CARTESIAN_POINT('',(16.2160625265911,-1.04967429885982,0.));
#9595=CARTESIAN_POINT('Origin',(0.,0.,0.));
#9596=CARTESIAN_POINT('',(18.8377966288376,-2.47738131311191,0.));
#9597=CARTESIAN_POINT('Ctrl Pts',(18.8377966288376,-2.47738131311191,0.));
#9598=CARTESIAN_POINT('Ctrl Pts',(18.6965496529788,-2.38389175781396,0.));
#9599=CARTESIAN_POINT('Ctrl Pts',(18.4751451900744,-2.24653249449211,0.));
#9600=CARTESIAN_POINT('Ctrl Pts',(18.1737325312257,-2.08026807216974,0.));
#9601=CARTESIAN_POINT('Ctrl Pts',(17.949326772361,-1.96717098182924,0.));
#9602=CARTESIAN_POINT('Ctrl Pts',(17.7407325407201,-1.87160676754275,0.));
#9603=CARTESIAN_POINT('Ctrl Pts',(17.548917731071,-1.7922273041827,0.));
#9604=CARTESIAN_POINT('Ctrl Pts',(17.3747717371572,-1.72763282051117,0.));
#9605=CARTESIAN_POINT('Ctrl Pts',(17.2191007779952,-1.67639424155261,0.));
#9606=CARTESIAN_POINT('Ctrl Pts',(17.0826338282621,-1.6370032466926,0.));
#9607=CARTESIAN_POINT('Ctrl Pts',(16.9659973771906,-1.60803840593143,0.));
#9608=CARTESIAN_POINT('Ctrl Pts',(16.8793055486399,-1.58971419725802,0.));
#9609=CARTESIAN_POINT('Ctrl Pts',(16.8195656763126,-1.57930034717563,0.));
#9610=CARTESIAN_POINT('Ctrl Pts',(16.7804505865492,-1.57225556404309,0.));
#9611=CARTESIAN_POINT('Ctrl Pts',(16.7455711436431,-1.56489594057215,0.));
#9612=CARTESIAN_POINT('Ctrl Pts',(16.6896454316358,-1.55162638755015,0.));
#9613=CARTESIAN_POINT('Ctrl Pts',(16.6138949491149,-1.5291889967686,0.));
#9614=CARTESIAN_POINT('Ctrl Pts',(16.5198135565977,-1.49051796169807,0.));
#9615=CARTESIAN_POINT('Ctrl Pts',(16.4279450992207,-1.43783746532129,0.));
#9616=CARTESIAN_POINT('Ctrl Pts',(16.3372938385016,-1.36201264541057,0.));
#9617=CARTESIAN_POINT('Ctrl Pts',(16.2452435266959,-1.23650382033374,0.));
#9618=CARTESIAN_POINT('Ctrl Pts',(16.2167242606458,-1.11994179848647,0.));
#9619=CARTESIAN_POINT('Ctrl Pts',(16.2160625265911,-1.04967429885982,0.));
#9620=CARTESIAN_POINT('',(18.6813621637973,-3.46506965370701,0.));
#9621=CARTESIAN_POINT('Origin',(0.,0.,0.));
#9622=CARTESIAN_POINT('',(15.7467591314704,-4.01273932064523,0.));
#9623=CARTESIAN_POINT('Ctrl Pts',(15.7467591314704,-4.01273932064523,0.));
#9624=CARTESIAN_POINT('Ctrl Pts',(15.7691023294921,-3.94611544431022,0.));
#9625=CARTESIAN_POINT('Ctrl Pts',(15.8322454089585,-3.8440713117564,0.));
#9626=CARTESIAN_POINT('Ctrl Pts',(15.958574817721,-3.75315043650002,0.));
#9627=CARTESIAN_POINT('Ctrl Pts',(16.0682204478862,-3.70904952755073,0.));
#9628=CARTESIAN_POINT('Ctrl Pts',(16.1718717115691,-3.68733631276642,0.));
#9629=CARTESIAN_POINT('Ctrl Pts',(16.2732984400115,-3.67963072201298,0.));
#9630=CARTESIAN_POINT('Ctrl Pts',(16.3522749650865,-3.68169968173262,0.));
#9631=CARTESIAN_POINT('Ctrl Pts',(16.409563995311,-3.68636158229546,0.));
#9632=CARTESIAN_POINT('Ctrl Pts',(16.4450105654963,-3.69014050504826,0.));
#9633=CARTESIAN_POINT('Ctrl Pts',(16.4843881842109,-3.6955277456176,0.));
#9634=CARTESIAN_POINT('Ctrl Pts',(16.5444222357228,-3.70408422142792,0.));
#9635=CARTESIAN_POINT('Ctrl Pts',(16.632533556064,-3.71344611165872,0.));
#9636=CARTESIAN_POINT('Ctrl Pts',(16.7524120409277,-3.72194155665406,0.));
#9637=CARTESIAN_POINT('Ctrl Pts',(16.8943723095674,-3.72664910094713,0.));
#9638=CARTESIAN_POINT('Ctrl Pts',(17.0582577813421,-3.72602328845455,0.));
#9639=CARTESIAN_POINT('Ctrl Pts',(17.2438412568379,-3.71840435546376,0.));
#9640=CARTESIAN_POINT('Ctrl Pts',(17.4507975846592,-3.70218403552949,0.));
#9641=CARTESIAN_POINT('Ctrl Pts',(17.6787134541915,-3.67575622931335,0.));
#9642=CARTESIAN_POINT('Ctrl Pts',(17.9270849363835,-3.63753969769582,0.));
#9643=CARTESIAN_POINT('Ctrl Pts',(18.265123941733,-3.57255446932205,0.));
#9644=CARTESIAN_POINT('Ctrl Pts',(18.5181384456163,-3.51033578853422,0.));
#9645=CARTESIAN_POINT('Ctrl Pts',(18.6813621637973,-3.46506965370701,0.));
#9646=CARTESIAN_POINT('',(15.0980247376579,-6.00933848448159,0.));
#9647=CARTESIAN_POINT('Origin',(0.,0.,0.));
#9648=CARTESIAN_POINT('',(17.1502563092003,-8.17732893607285,0.));
#9649=CARTESIAN_POINT('Ctrl Pts',(17.1502563092003,-8.17732893607285,0.));
#9650=CARTESIAN_POINT('Ctrl Pts',(17.0448123137865,-8.04476736935674,0.));
#9651=CARTESIAN_POINT('Ctrl Pts',(16.8766905033057,-7.84571320523309,0.));
#9652=CARTESIAN_POINT('Ctrl Pts',(16.6414085620714,-7.59444470905136,0.));
#9653=CARTESIAN_POINT('Ctrl Pts',(16.4629349257385,-7.41753779118421,0.));
#9654=CARTESIAN_POINT('Ctrl Pts',(16.2940809887434,-7.26219165995679,0.));
#9655=CARTESIAN_POINT('Ctrl Pts',(16.1361838672874,-7.12742326811383,0.));
#9656=CARTESIAN_POINT('Ctrl Pts',(15.9905219781863,-7.01217619187962,0.));
#9657=CARTESIAN_POINT('Ctrl Pts',(15.8583036897433,-6.91534043556369,0.));
#9658=CARTESIAN_POINT('Ctrl Pts',(15.7406883947777,-6.83570676658069,0.));
#9659=CARTESIAN_POINT('Ctrl Pts',(15.6387111659832,-6.77211692048663,0.));
#9660=CARTESIAN_POINT('Ctrl Pts',(15.5619248294191,-6.72790031412624,0.));
#9661=CARTESIAN_POINT('Ctrl Pts',(15.5083268912119,-6.69953551835472,0.));
#9662=CARTESIAN_POINT('Ctrl Pts',(15.4733031879166,-6.68074830397725,0.));
#9663=CARTESIAN_POINT('Ctrl Pts',(15.4424051151807,-6.66297054550541,0.));
#9664=CARTESIAN_POINT('Ctrl Pts',(15.3933171197393,-6.63306845520276,0.));
#9665=CARTESIAN_POINT('Ctrl Pts',(15.3282076647862,-6.58832104206022,0.));
#9666=CARTESIAN_POINT('Ctrl Pts',(15.2506809503975,-6.52246995302226,0.));
#9667=CARTESIAN_POINT('Ctrl Pts',(15.1795880240196,-6.44397890908496,0.));
#9668=CARTESIAN_POINT('Ctrl Pts',(15.1168047097501,-6.34385243988822,0.));
#9669=CARTESIAN_POINT('Ctrl Pts',(15.0680440207731,-6.1960413432609,0.));
#9670=CARTESIAN_POINT('Ctrl Pts',(15.0769402326058,-6.07637133495394,0.));
#9671=CARTESIAN_POINT('Ctrl Pts',(15.0980247376579,-6.00933848448159,0.));
#9672=CARTESIAN_POINT('',(16.6962658094608,-9.06833546026116,0.));
#9673=CARTESIAN_POINT('Origin',(0.,0.,0.));
#9674=CARTESIAN_POINT('',(13.7360532384392,-8.68235805704669,0.));
#9675=CARTESIAN_POINT('Ctrl Pts',(13.7360532384392,-8.68235805704669,0.));
#9676=CARTESIAN_POINT('Ctrl Pts',(13.7778907925313,-8.62589941321482,0.));
#9677=CARTESIAN_POINT('Ctrl Pts',(13.8694768008521,-8.54836196063209,0.));
#9678=CARTESIAN_POINT('Ctrl Pts',(14.0177193038531,-8.50092900394922,0.));
#9679=CARTESIAN_POINT('Ctrl Pts',(14.1356264252377,-8.49286891019844,0.));
#9680=CARTESIAN_POINT('Ctrl Pts',(14.2409143873564,-8.50424841775457,0.));
#9681=CARTESIAN_POINT('Ctrl Pts',(14.3397580968626,-8.52826254822916,0.));
#9682=CARTESIAN_POINT('Ctrl Pts',(14.4142298919554,-8.55463533425733,0.));
#9683=CARTESIAN_POINT('Ctrl Pts',(14.4672743909627,-8.57677234909657,0.));
#9684=CARTESIAN_POINT('Ctrl Pts',(14.4998183311667,-8.59131991078477,0.));
#9685=CARTESIAN_POINT('Ctrl Pts',(14.5356039231527,-8.6086118344139,0.));
#9686=CARTESIAN_POINT('Ctrl Pts',(14.5900556026053,-8.63530106864818,0.));
#9687=CARTESIAN_POINT('Ctrl Pts',(14.6709614647944,-8.67143265073928,0.));
#9688=CARTESIAN_POINT('Ctrl Pts',(14.7823474421092,-8.71655678814373,0.));
#9689=CARTESIAN_POINT('Ctrl Pts',(14.9159049694657,-8.7649020643551,0.));
#9690=CARTESIAN_POINT('Ctrl Pts',(15.0719627020186,-8.81495027721557,0.));
#9691=CARTESIAN_POINT('Ctrl Pts',(15.2508174554788,-8.86505268915084,0.));
#9692=CARTESIAN_POINT('Ctrl Pts',(15.4526569741556,-8.91357927057117,0.));
#9693=CARTESIAN_POINT('Ctrl Pts',(15.6775844882862,-8.95887481023116,0.));
#9694=CARTESIAN_POINT('Ctrl Pts',(15.9256093626227,-8.99927973772153,0.));
#9695=CARTESIAN_POINT('Ctrl Pts',(16.2671851013731,-9.04193491022831,0.));
#9696=CARTESIAN_POINT('Ctrl Pts',(16.5270428237395,-9.06094720995305,0.));
#9697=CARTESIAN_POINT('Ctrl Pts',(16.6962658094608,-9.06833546026116,0.));
#9698=CARTESIAN_POINT('',(12.5020870932787,-10.3807667497191,0.));
#9699=CARTESIAN_POINT('Origin',(0.,0.,0.));
#9700=CARTESIAN_POINT('',(13.7839294091565,-13.0768226279701,0.));
#9701=CARTESIAN_POINT('Ctrl Pts',(13.7839294091565,-13.0768226279701,0.));
#9702=CARTESIAN_POINT('Ctrl Pts',(13.7246099871302,-12.9181650995967,0.));
#9703=CARTESIAN_POINT('Ctrl Pts',(13.6262277632565,-12.6769008431476,0.));
#9704=CARTESIAN_POINT('Ctrl Pts',(13.4801075753502,-12.3652241842034,0.));
#9705=CARTESIAN_POINT('Ctrl Pts',(13.3650363045723,-12.1418243205134,0.));
#9706=CARTESIAN_POINT('Ctrl Pts',(13.2524512620508,-11.9419026340297,0.));
#9707=CARTESIAN_POINT('Ctrl Pts',(13.1439278991698,-11.764937382884,0.));
#9708=CARTESIAN_POINT('Ctrl Pts',(13.0410085154728,-11.6103189008825,0.));
#9709=CARTESIAN_POINT('Ctrl Pts',(12.9451853450404,-11.4773649257318,0.));
#9710=CARTESIAN_POINT('Ctrl Pts',(12.8579347093876,-11.3652836809863,0.));
#9711=CARTESIAN_POINT('Ctrl Pts',(12.7805989445416,-11.2732934467515,0.));
#9712=CARTESIAN_POINT('Ctrl Pts',(12.7212344815888,-11.2075126722099,0.));
#9713=CARTESIAN_POINT('Ctrl Pts',(12.6790250171322,-11.1639734745885,0.));
#9714=CARTESIAN_POINT('Ctrl Pts',(12.6515210644081,-11.1352828524076,0.));
#9715=CARTESIAN_POINT('Ctrl Pts',(12.6276288804813,-11.108827169799,0.));
#9716=CARTESIAN_POINT('Ctrl Pts',(12.5901836766158,-11.0652195671547,0.));
#9717=CARTESIAN_POINT('Ctrl Pts',(12.5420886163255,-11.0025423202231,0.));
#9718=CARTESIAN_POINT('Ctrl Pts',(12.48870543503,-10.9159571406243,0.));
#9719=CARTESIAN_POINT('Ctrl Pts',(12.4453471106188,-10.8193387993863,0.));
#9720=CARTESIAN_POINT('Ctrl Pts',(12.4165774110367,-10.7047117573306,0.));
#9721=CARTESIAN_POINT('Ctrl Pts',(12.4158793808611,-10.5490671691512,0.));
#9722=CARTESIAN_POINT('Ctrl Pts',(12.4613202473788,-10.4380033085876,0.));
#9723=CARTESIAN_POINT('Ctrl Pts',(12.5020870932787,-10.3807667497191,0.));
#9724=CARTESIAN_POINT('',(13.07682262797,-13.7839294091566,0.));
#9725=CARTESIAN_POINT('Origin',(0.,1.10390771809154E-15,0.));
#9726=CARTESIAN_POINT('',(10.3807667497191,-12.5020870932787,0.));
#9727=CARTESIAN_POINT('Ctrl Pts',(10.3807667497191,-12.5020870932787,0.));
#9728=CARTESIAN_POINT('Ctrl Pts',(10.4380033085876,-12.4613202473788,0.));
#9729=CARTESIAN_POINT('Ctrl Pts',(10.5490671691512,-12.4158793808611,0.));
#9730=CARTESIAN_POINT('Ctrl Pts',(10.7047117573306,-12.4165774110367,0.));
#9731=CARTESIAN_POINT('Ctrl Pts',(10.8193387993863,-12.4453471106188,0.));
#9732=CARTESIAN_POINT('Ctrl Pts',(10.9159571406243,-12.48870543503,0.));
#9733=CARTESIAN_POINT('Ctrl Pts',(11.0025423202231,-12.5420886163255,0.));
#9734=CARTESIAN_POINT('Ctrl Pts',(11.0652195671547,-12.5901836766158,0.));
#9735=CARTESIAN_POINT('Ctrl Pts',(11.1088271697991,-12.6276288804813,0.));
#9736=CARTESIAN_POINT('Ctrl Pts',(11.1352828524077,-12.651521064408,0.));
#9737=CARTESIAN_POINT('Ctrl Pts',(11.1639734745885,-12.6790250171322,0.));
#9738=CARTESIAN_POINT('Ctrl Pts',(11.2075126722099,-12.7212344815888,0.));
#9739=CARTESIAN_POINT('Ctrl Pts',(11.2732934467515,-12.7805989445416,0.));
#9740=CARTESIAN_POINT('Ctrl Pts',(11.3652836809863,-12.8579347093876,0.));
#9741=CARTESIAN_POINT('Ctrl Pts',(11.4773649257318,-12.9451853450404,0.));
#9742=CARTESIAN_POINT('Ctrl Pts',(11.6103189008825,-13.0410085154727,0.));
#9743=CARTESIAN_POINT('Ctrl Pts',(11.764937382884,-13.1439278991698,0.));
#9744=CARTESIAN_POINT('Ctrl Pts',(11.9419026340297,-13.2524512620507,0.));
#9745=CARTESIAN_POINT('Ctrl Pts',(12.1418243205134,-13.3650363045724,0.));
#9746=CARTESIAN_POINT('Ctrl Pts',(12.3652241842034,-13.4801075753502,0.));
#9747=CARTESIAN_POINT('Ctrl Pts',(12.6769008431476,-13.6262277632565,0.));
#9748=CARTESIAN_POINT('Ctrl Pts',(12.9181650995967,-13.7246099871303,0.));
#9749=CARTESIAN_POINT('Ctrl Pts',(13.07682262797,-13.7839294091566,0.));
#9750=CARTESIAN_POINT('',(8.68235805704667,-13.7360532384392,0.));
#9751=CARTESIAN_POINT('Origin',(0.,0.,0.));
#9752=CARTESIAN_POINT('',(9.06833546026109,-16.6962658094609,0.));
#9753=CARTESIAN_POINT('Ctrl Pts',(9.06833546026109,-16.6962658094609,0.));
#9754=CARTESIAN_POINT('Ctrl Pts',(9.06094720995301,-16.5270428237395,0.));
#9755=CARTESIAN_POINT('Ctrl Pts',(9.0419349102283,-16.267185101373,0.));
#9756=CARTESIAN_POINT('Ctrl Pts',(8.99927973772149,-15.9256093626227,0.));
#9757=CARTESIAN_POINT('Ctrl Pts',(8.95887481023114,-15.6775844882862,0.));
#9758=CARTESIAN_POINT('Ctrl Pts',(8.91357927057119,-15.4526569741556,0.));
#9759=CARTESIAN_POINT('Ctrl Pts',(8.8650526891508,-15.2508174554787,0.));
#9760=CARTESIAN_POINT('Ctrl Pts',(8.81495027721559,-15.0719627020186,0.));
#9761=CARTESIAN_POINT('Ctrl Pts',(8.76490206435508,-14.9159049694657,0.));
#9762=CARTESIAN_POINT('Ctrl Pts',(8.7165567881437,-14.7823474421092,0.));
#9763=CARTESIAN_POINT('Ctrl Pts',(8.67143265073927,-14.6709614647944,0.));
#9764=CARTESIAN_POINT('Ctrl Pts',(8.63530106864817,-14.5900556026053,0.));
#9765=CARTESIAN_POINT('Ctrl Pts',(8.60861183441386,-14.5356039231526,0.));
#9766=CARTESIAN_POINT('Ctrl Pts',(8.59131991078477,-14.4998183311667,0.));
#9767=CARTESIAN_POINT('Ctrl Pts',(8.57677234909656,-14.4672743909626,0.));
#9768=CARTESIAN_POINT('Ctrl Pts',(8.55463533425731,-14.4142298919554,0.));
#9769=CARTESIAN_POINT('Ctrl Pts',(8.52826254822914,-14.3397580968625,0.));
#9770=CARTESIAN_POINT('Ctrl Pts',(8.50424841775455,-14.2409143873564,0.));
#9771=CARTESIAN_POINT('Ctrl Pts',(8.49286891019841,-14.1356264252376,0.));
#9772=CARTESIAN_POINT('Ctrl Pts',(8.50092900394917,-14.0177193038531,0.));
#9773=CARTESIAN_POINT('Ctrl Pts',(8.54836196063206,-13.8694768008521,0.));
#9774=CARTESIAN_POINT('Ctrl Pts',(8.62589941321478,-13.7778907925312,0.));
#9775=CARTESIAN_POINT('Ctrl Pts',(8.68235805704667,-13.7360532384392,0.));
#9776=CARTESIAN_POINT('',(8.17732893607279,-17.1502563092004,0.));
#9777=CARTESIAN_POINT('Origin',(0.,0.,0.));
#9778=CARTESIAN_POINT('',(6.00933848448151,-15.0980247376579,0.));
#9779=CARTESIAN_POINT('Ctrl Pts',(6.00933848448151,-15.0980247376579,0.));
#9780=CARTESIAN_POINT('Ctrl Pts',(6.07637133495396,-15.0769402326058,0.));
#9781=CARTESIAN_POINT('Ctrl Pts',(6.1960413432609,-15.0680440207731,0.));
#9782=CARTESIAN_POINT('Ctrl Pts',(6.34385243988821,-15.1168047097502,0.));
#9783=CARTESIAN_POINT('Ctrl Pts',(6.44397890908497,-15.1795880240196,0.));
#9784=CARTESIAN_POINT('Ctrl Pts',(6.52246995302229,-15.2506809503975,0.));
#9785=CARTESIAN_POINT('Ctrl Pts',(6.58832104206024,-15.3282076647862,0.));
#9786=CARTESIAN_POINT('Ctrl Pts',(6.63306845520277,-15.3933171197393,0.));
#9787=CARTESIAN_POINT('Ctrl Pts',(6.66297054550544,-15.4424051151807,0.));
#9788=CARTESIAN_POINT('Ctrl Pts',(6.68074830397727,-15.4733031879166,0.));
#9789=CARTESIAN_POINT('Ctrl Pts',(6.69953551835471,-15.5083268912119,0.));
#9790=CARTESIAN_POINT('Ctrl Pts',(6.72790031412625,-15.5619248294191,0.));
#9791=CARTESIAN_POINT('Ctrl Pts',(6.77211692048664,-15.6387111659832,0.));
#9792=CARTESIAN_POINT('Ctrl Pts',(6.83570676658069,-15.7406883947778,0.));
#9793=CARTESIAN_POINT('Ctrl Pts',(6.91534043556371,-15.8583036897433,0.));
#9794=CARTESIAN_POINT('Ctrl Pts',(7.01217619187964,-15.9905219781863,0.));
#9795=CARTESIAN_POINT('Ctrl Pts',(7.12742326811382,-16.1361838672874,0.));
#9796=CARTESIAN_POINT('Ctrl Pts',(7.2621916599568,-16.2940809887434,0.));
#9797=CARTESIAN_POINT('Ctrl Pts',(7.41753779118422,-16.4629349257385,0.));
#9798=CARTESIAN_POINT('Ctrl Pts',(7.59444470905135,-16.6414085620714,0.));
#9799=CARTESIAN_POINT('Ctrl Pts',(7.84571320523309,-16.8766905033058,0.));
#9800=CARTESIAN_POINT('Ctrl Pts',(8.04476736935673,-17.0448123137865,0.));
#9801=CARTESIAN_POINT('Ctrl Pts',(8.17732893607279,-17.1502563092004,0.));
#9802=CARTESIAN_POINT('',(4.01273932064523,-15.7467591314704,0.));
#9803=CARTESIAN_POINT('Origin',(0.,0.,0.));
#9804=CARTESIAN_POINT('',(3.46506965370692,-18.6813621637974,0.));
#9805=CARTESIAN_POINT('Ctrl Pts',(3.46506965370692,-18.6813621637974,0.));
#9806=CARTESIAN_POINT('Ctrl Pts',(3.51033578853419,-18.5181384456162,0.));
#9807=CARTESIAN_POINT('Ctrl Pts',(3.57255446932203,-18.2651239417329,0.));
#9808=CARTESIAN_POINT('Ctrl Pts',(3.63753969769579,-17.9270849363835,0.));
#9809=CARTESIAN_POINT('Ctrl Pts',(3.67575622931334,-17.6787134541915,0.));
#9810=CARTESIAN_POINT('Ctrl Pts',(3.7021840355295,-17.4507975846592,0.));
#9811=CARTESIAN_POINT('Ctrl Pts',(3.71840435546372,-17.2438412568379,0.));
#9812=CARTESIAN_POINT('Ctrl Pts',(3.72602328845457,-17.0582577813421,0.));
#9813=CARTESIAN_POINT('Ctrl Pts',(3.72664910094712,-16.8943723095674,0.));
#9814=CARTESIAN_POINT('Ctrl Pts',(3.72194155665404,-16.7524120409277,0.));
#9815=CARTESIAN_POINT('Ctrl Pts',(3.71344611165872,-16.632533556064,0.));
#9816=CARTESIAN_POINT('Ctrl Pts',(3.70408422142791,-16.5444222357228,0.));
#9817=CARTESIAN_POINT('Ctrl Pts',(3.69552774561757,-16.4843881842109,0.));
#9818=CARTESIAN_POINT('Ctrl Pts',(3.69014050504827,-16.4450105654963,0.));
#9819=CARTESIAN_POINT('Ctrl Pts',(3.68636158229547,-16.409563995311,0.));
#9820=CARTESIAN_POINT('Ctrl Pts',(3.68169968173261,-16.3522749650865,0.));
#9821=CARTESIAN_POINT('Ctrl Pts',(3.67963072201297,-16.2732984400115,0.));
#9822=CARTESIAN_POINT('Ctrl Pts',(3.68733631276642,-16.1718717115691,0.));
#9823=CARTESIAN_POINT('Ctrl Pts',(3.70904952755071,-16.0682204478862,0.));
#9824=CARTESIAN_POINT('Ctrl Pts',(3.75315043649999,-15.958574817721,0.));
#9825=CARTESIAN_POINT('Ctrl Pts',(3.84407131175639,-15.8322454089585,0.));
#9826=CARTESIAN_POINT('Ctrl Pts',(3.94611544431021,-15.7691023294921,0.));
#9827=CARTESIAN_POINT('Ctrl Pts',(4.01273932064523,-15.7467591314704,0.));
#9828=CARTESIAN_POINT('',(2.47738131311187,-18.8377966288376,0.));
#9829=CARTESIAN_POINT('Origin',(0.,0.,0.));
#9830=CARTESIAN_POINT('',(1.04967429885974,-16.2160625265911,0.));
#9831=CARTESIAN_POINT('Ctrl Pts',(1.04967429885974,-16.2160625265911,0.));
#9832=CARTESIAN_POINT('Ctrl Pts',(1.11994179848648,-16.2167242606459,0.));
#9833=CARTESIAN_POINT('Ctrl Pts',(1.23650382033375,-16.2452435266959,0.));
#9834=CARTESIAN_POINT('Ctrl Pts',(1.36201264541055,-16.3372938385016,0.));
#9835=CARTESIAN_POINT('Ctrl Pts',(1.4378374653213,-16.4279450992208,0.));
#9836=CARTESIAN_POINT('Ctrl Pts',(1.4905179616981,-16.5198135565978,0.));
#9837=CARTESIAN_POINT('Ctrl Pts',(1.52918899676862,-16.6138949491149,0.));
#9838=CARTESIAN_POINT('Ctrl Pts',(1.55162638755016,-16.6896454316359,0.));
#9839=CARTESIAN_POINT('Ctrl Pts',(1.56489594057218,-16.7455711436431,0.));
#9840=CARTESIAN_POINT('Ctrl Pts',(1.57225556404312,-16.7804505865492,0.));
#9841=CARTESIAN_POINT('Ctrl Pts',(1.57930034717562,-16.8195656763126,0.));
#9842=CARTESIAN_POINT('Ctrl Pts',(1.58971419725804,-16.8793055486399,0.));
#9843=CARTESIAN_POINT('Ctrl Pts',(1.60803840593144,-16.9659973771906,0.));
#9844=CARTESIAN_POINT('Ctrl Pts',(1.6370032466926,-17.0826338282622,0.));
#9845=CARTESIAN_POINT('Ctrl Pts',(1.67639424155263,-17.2191007779953,0.));
#9846=CARTESIAN_POINT('Ctrl Pts',(1.72763282051121,-17.3747717371572,0.));
#9847=CARTESIAN_POINT('Ctrl Pts',(1.79222730418269,-17.548917731071,0.));
#9848=CARTESIAN_POINT('Ctrl Pts',(1.87160676754277,-17.7407325407201,0.));
#9849=CARTESIAN_POINT('Ctrl Pts',(1.96717098182925,-17.949326772361,0.));
#9850=CARTESIAN_POINT('Ctrl Pts',(2.08026807216972,-18.1737325312257,0.));
#9851=CARTESIAN_POINT('Ctrl Pts',(2.2465324944921,-18.4751451900744,0.));
#9852=CARTESIAN_POINT('Ctrl Pts',(2.38389175781394,-18.6965496529788,0.));
#9853=CARTESIAN_POINT('Ctrl Pts',(2.47738131311187,-18.8377966288376,0.));
#9854=CARTESIAN_POINT('',(-1.04967429885986,-16.2160625265911,0.));
#9855=CARTESIAN_POINT('Origin',(0.,0.,0.));
#9856=CARTESIAN_POINT('',(-2.47738131311198,-18.8377966288376,0.));
#9857=CARTESIAN_POINT('Ctrl Pts',(-2.47738131311198,-18.8377966288376,0.));
#9858=CARTESIAN_POINT('Ctrl Pts',(-2.38389175781398,-18.6965496529788,0.));
#9859=CARTESIAN_POINT('Ctrl Pts',(-2.24653249449213,-18.4751451900744,0.));
#9860=CARTESIAN_POINT('Ctrl Pts',(-2.08026807216976,-18.1737325312257,0.));
#9861=CARTESIAN_POINT('Ctrl Pts',(-1.96717098182926,-17.949326772361,0.));
#9862=CARTESIAN_POINT('Ctrl Pts',(-1.87160676754278,-17.7407325407201,0.));
#9863=CARTESIAN_POINT('Ctrl Pts',(-1.79222730418273,-17.548917731071,0.));
#9864=CARTESIAN_POINT('Ctrl Pts',(-1.7276328205112,-17.3747717371572,0.));
#9865=CARTESIAN_POINT('Ctrl Pts',(-1.67639424155264,-17.2191007779952,0.));
#9866=CARTESIAN_POINT('Ctrl Pts',(-1.63700324669264,-17.0826338282621,0.));
#9867=CARTESIAN_POINT('Ctrl Pts',(-1.60803840593146,-16.9659973771906,0.));
#9868=CARTESIAN_POINT('Ctrl Pts',(-1.58971419725806,-16.8793055486399,0.));
#9869=CARTESIAN_POINT('Ctrl Pts',(-1.57930034717566,-16.8195656763126,0.));
#9870=CARTESIAN_POINT('Ctrl Pts',(-1.57225556404312,-16.7804505865492,0.));
#9871=CARTESIAN_POINT('Ctrl Pts',(-1.56489594057218,-16.7455711436431,0.));
#9872=CARTESIAN_POINT('Ctrl Pts',(-1.55162638755018,-16.6896454316358,0.));
#9873=CARTESIAN_POINT('Ctrl Pts',(-1.52918899676863,-16.6138949491149,0.));
#9874=CARTESIAN_POINT('Ctrl Pts',(-1.49051796169811,-16.5198135565977,0.));
#9875=CARTESIAN_POINT('Ctrl Pts',(-1.43783746532133,-16.4279450992207,0.));
#9876=CARTESIAN_POINT('Ctrl Pts',(-1.3620126454106,-16.3372938385016,0.));
#9877=CARTESIAN_POINT('Ctrl Pts',(-1.23650382033378,-16.2452435266959,0.));
#9878=CARTESIAN_POINT('Ctrl Pts',(-1.1199417984865,-16.2167242606458,0.));
#9879=CARTESIAN_POINT('Ctrl Pts',(-1.04967429885986,-16.2160625265911,0.));
#9880=CARTESIAN_POINT('',(-3.46506965370701,-18.6813621637973,0.));
#9881=CARTESIAN_POINT('Origin',(0.,0.,0.));
#9882=CARTESIAN_POINT('',(-4.01273932064531,-15.7467591314704,0.));
#9883=CARTESIAN_POINT('Ctrl Pts',(-4.01273932064531,-15.7467591314704,0.));
#9884=CARTESIAN_POINT('Ctrl Pts',(-3.94611544431022,-15.7691023294921,0.));
#9885=CARTESIAN_POINT('Ctrl Pts',(-3.8440713117564,-15.8322454089585,0.));
#9886=CARTESIAN_POINT('Ctrl Pts',(-3.75315043650002,-15.958574817721,0.));
#9887=CARTESIAN_POINT('Ctrl Pts',(-3.70904952755073,-16.0682204478862,0.));
#9888=CARTESIAN_POINT('Ctrl Pts',(-3.68733631276642,-16.1718717115691,0.));
#9889=CARTESIAN_POINT('Ctrl Pts',(-3.67963072201298,-16.2732984400115,0.));
#9890=CARTESIAN_POINT('Ctrl Pts',(-3.68169968173261,-16.3522749650865,0.));
#9891=CARTESIAN_POINT('Ctrl Pts',(-3.68636158229546,-16.409563995311,0.));
#9892=CARTESIAN_POINT('Ctrl Pts',(-3.69014050504826,-16.4450105654963,0.));
#9893=CARTESIAN_POINT('Ctrl Pts',(-3.6955277456176,-16.4843881842109,0.));
#9894=CARTESIAN_POINT('Ctrl Pts',(-3.70408422142792,-16.5444222357228,0.));
#9895=CARTESIAN_POINT('Ctrl Pts',(-3.71344611165872,-16.632533556064,0.));
#9896=CARTESIAN_POINT('Ctrl Pts',(-3.72194155665407,-16.7524120409277,0.));
#9897=CARTESIAN_POINT('Ctrl Pts',(-3.72664910094713,-16.8943723095674,0.));
#9898=CARTESIAN_POINT('Ctrl Pts',(-3.72602328845455,-17.0582577813421,0.));
#9899=CARTESIAN_POINT('Ctrl Pts',(-3.71840435546375,-17.2438412568379,0.));
#9900=CARTESIAN_POINT('Ctrl Pts',(-3.70218403552949,-17.4507975846592,0.));
#9901=CARTESIAN_POINT('Ctrl Pts',(-3.67575622931335,-17.6787134541915,0.));
#9902=CARTESIAN_POINT('Ctrl Pts',(-3.63753969769582,-17.9270849363835,0.));
#9903=CARTESIAN_POINT('Ctrl Pts',(-3.57255446932205,-18.265123941733,0.));
#9904=CARTESIAN_POINT('Ctrl Pts',(-3.51033578853422,-18.5181384456163,0.));
#9905=CARTESIAN_POINT('Ctrl Pts',(-3.46506965370701,-18.6813621637973,0.));
#9906=CARTESIAN_POINT('',(-6.0093384844816,-15.0980247376578,0.));
#9907=CARTESIAN_POINT('Origin',(0.,0.,0.));
#9908=CARTESIAN_POINT('',(-8.17732893607292,-17.1502563092003,0.));
#9909=CARTESIAN_POINT('Ctrl Pts',(-8.17732893607292,-17.1502563092003,0.));
#9910=CARTESIAN_POINT('Ctrl Pts',(-8.04476736935674,-17.0448123137865,0.));
#9911=CARTESIAN_POINT('Ctrl Pts',(-7.8457132052331,-16.8766905033057,0.));
#9912=CARTESIAN_POINT('Ctrl Pts',(-7.59444470905137,-16.6414085620714,0.));
#9913=CARTESIAN_POINT('Ctrl Pts',(-7.41753779118422,-16.4629349257385,0.));
#9914=CARTESIAN_POINT('Ctrl Pts',(-7.2621916599568,-16.2940809887434,0.));
#9915=CARTESIAN_POINT('Ctrl Pts',(-7.12742326811384,-16.1361838672874,0.));
#9916=CARTESIAN_POINT('Ctrl Pts',(-7.01217619187963,-15.9905219781863,0.));
#9917=CARTESIAN_POINT('Ctrl Pts',(-6.9153404355637,-15.8583036897432,0.));
#9918=CARTESIAN_POINT('Ctrl Pts',(-6.8357067665807,-15.7406883947777,0.));
#9919=CARTESIAN_POINT('Ctrl Pts',(-6.77211692048664,-15.6387111659832,0.));
#9920=CARTESIAN_POINT('Ctrl Pts',(-6.72790031412625,-15.5619248294191,0.));
#9921=CARTESIAN_POINT('Ctrl Pts',(-6.69953551835473,-15.5083268912118,0.));
#9922=CARTESIAN_POINT('Ctrl Pts',(-6.68074830397727,-15.4733031879166,0.));
#9923=CARTESIAN_POINT('Ctrl Pts',(-6.66297054550543,-15.4424051151807,0.));
#9924=CARTESIAN_POINT('Ctrl Pts',(-6.63306845520277,-15.3933171197393,0.));
#9925=CARTESIAN_POINT('Ctrl Pts',(-6.58832104206024,-15.3282076647861,0.));
#9926=CARTESIAN_POINT('Ctrl Pts',(-6.52246995302227,-15.2506809503975,0.));
#9927=CARTESIAN_POINT('Ctrl Pts',(-6.44397890908497,-15.1795880240196,0.));
#9928=CARTESIAN_POINT('Ctrl Pts',(-6.34385243988824,-15.1168047097501,0.));
#9929=CARTESIAN_POINT('Ctrl Pts',(-6.19604134326091,-15.0680440207731,0.));
#9930=CARTESIAN_POINT('Ctrl Pts',(-6.07637133495395,-15.0769402326058,0.));
#9931=CARTESIAN_POINT('Ctrl Pts',(-6.0093384844816,-15.0980247376578,0.));
#9932=CARTESIAN_POINT('',(-9.06833546026116,-16.6962658094608,0.));
#9933=CARTESIAN_POINT('Origin',(0.,0.,0.));
#9934=CARTESIAN_POINT('',(-8.68235805704677,-13.7360532384392,0.));
#9935=CARTESIAN_POINT('Ctrl Pts',(-8.68235805704677,-13.7360532384392,0.));
#9936=CARTESIAN_POINT('Ctrl Pts',(-8.62589941321481,-13.7778907925313,0.));
#9937=CARTESIAN_POINT('Ctrl Pts',(-8.54836196063208,-13.8694768008521,0.));
#9938=CARTESIAN_POINT('Ctrl Pts',(-8.50092900394921,-14.0177193038531,0.));
#9939=CARTESIAN_POINT('Ctrl Pts',(-8.49286891019844,-14.1356264252377,0.));
#9940=CARTESIAN_POINT('Ctrl Pts',(-8.50424841775456,-14.2409143873564,0.));
#9941=CARTESIAN_POINT('Ctrl Pts',(-8.52826254822915,-14.3397580968626,0.));
#9942=CARTESIAN_POINT('Ctrl Pts',(-8.55463533425732,-14.4142298919555,0.));
#9943=CARTESIAN_POINT('Ctrl Pts',(-8.57677234909656,-14.4672743909627,0.));
#9944=CARTESIAN_POINT('Ctrl Pts',(-8.59131991078476,-14.4998183311667,0.));
#9945=CARTESIAN_POINT('Ctrl Pts',(-8.6086118344139,-14.5356039231527,0.));
#9946=CARTESIAN_POINT('Ctrl Pts',(-8.63530106864818,-14.5900556026053,0.));
#9947=CARTESIAN_POINT('Ctrl Pts',(-8.67143265073928,-14.6709614647944,0.));
#9948=CARTESIAN_POINT('Ctrl Pts',(-8.71655678814373,-14.7823474421093,0.));
#9949=CARTESIAN_POINT('Ctrl Pts',(-8.76490206435509,-14.9159049694657,0.));
#9950=CARTESIAN_POINT('Ctrl Pts',(-8.81495027721557,-15.0719627020186,0.));
#9951=CARTESIAN_POINT('Ctrl Pts',(-8.86505268915084,-15.2508174554788,0.));
#9952=CARTESIAN_POINT('Ctrl Pts',(-8.91357927057117,-15.4526569741556,0.));
#9953=CARTESIAN_POINT('Ctrl Pts',(-8.95887481023116,-15.6775844882862,0.));
#9954=CARTESIAN_POINT('Ctrl Pts',(-8.99927973772154,-15.9256093626227,0.));
#9955=CARTESIAN_POINT('Ctrl Pts',(-9.04193491022832,-16.2671851013731,0.));
#9956=CARTESIAN_POINT('Ctrl Pts',(-9.06094720995306,-16.5270428237395,0.));
#9957=CARTESIAN_POINT('Ctrl Pts',(-9.06833546026116,-16.6962658094608,0.));
#9958=CARTESIAN_POINT('',(-10.3807667497191,-12.5020870932787,0.));
#9959=CARTESIAN_POINT('Origin',(0.,0.,0.));
#9960=CARTESIAN_POINT('',(-13.0768226279701,-13.7839294091565,0.));
#9961=CARTESIAN_POINT('Ctrl Pts',(-13.0768226279701,-13.7839294091565,0.));
#9962=CARTESIAN_POINT('Ctrl Pts',(-12.9181650995967,-13.7246099871302,0.));
#9963=CARTESIAN_POINT('Ctrl Pts',(-12.6769008431476,-13.6262277632565,0.));
#9964=CARTESIAN_POINT('Ctrl Pts',(-12.3652241842034,-13.4801075753502,0.));
#9965=CARTESIAN_POINT('Ctrl Pts',(-12.1418243205134,-13.3650363045723,0.));
#9966=CARTESIAN_POINT('Ctrl Pts',(-11.9419026340297,-13.2524512620508,0.));
#9967=CARTESIAN_POINT('Ctrl Pts',(-11.764937382884,-13.1439278991698,0.));
#9968=CARTESIAN_POINT('Ctrl Pts',(-11.6103189008825,-13.0410085154728,0.));
#9969=CARTESIAN_POINT('Ctrl Pts',(-11.4773649257318,-12.9451853450404,0.));
#9970=CARTESIAN_POINT('Ctrl Pts',(-11.3652836809863,-12.8579347093876,0.));
#9971=CARTESIAN_POINT('Ctrl Pts',(-11.2732934467515,-12.7805989445416,0.));
#9972=CARTESIAN_POINT('Ctrl Pts',(-11.2075126722099,-12.7212344815888,0.));
#9973=CARTESIAN_POINT('Ctrl Pts',(-11.1639734745886,-12.6790250171322,0.));
#9974=CARTESIAN_POINT('Ctrl Pts',(-11.1352828524077,-12.651521064408,0.));
#9975=CARTESIAN_POINT('Ctrl Pts',(-11.1088271697991,-12.6276288804813,0.));
#9976=CARTESIAN_POINT('Ctrl Pts',(-11.0652195671547,-12.5901836766158,0.));
#9977=CARTESIAN_POINT('Ctrl Pts',(-11.0025423202231,-12.5420886163255,0.));
#9978=CARTESIAN_POINT('Ctrl Pts',(-10.9159571406243,-12.48870543503,0.));
#9979=CARTESIAN_POINT('Ctrl Pts',(-10.8193387993863,-12.4453471106187,0.));
#9980=CARTESIAN_POINT('Ctrl Pts',(-10.7047117573307,-12.4165774110367,0.));
#9981=CARTESIAN_POINT('Ctrl Pts',(-10.5490671691512,-12.4158793808611,0.));
#9982=CARTESIAN_POINT('Ctrl Pts',(-10.4380033085876,-12.4613202473787,0.));
#9983=CARTESIAN_POINT('Ctrl Pts',(-10.3807667497191,-12.5020870932787,0.));
#9984=CARTESIAN_POINT('',(-13.7839294091566,-13.07682262797,0.));
#9985=CARTESIAN_POINT('Origin',(0.,0.,0.));
#9986=CARTESIAN_POINT('',(-12.5020870932788,-10.380766749719,0.));
#9987=CARTESIAN_POINT('Ctrl Pts',(-12.5020870932788,-10.380766749719,0.));
#9988=CARTESIAN_POINT('Ctrl Pts',(-12.4613202473788,-10.4380033085876,0.));
#9989=CARTESIAN_POINT('Ctrl Pts',(-12.4158793808611,-10.5490671691512,0.));
#9990=CARTESIAN_POINT('Ctrl Pts',(-12.4165774110367,-10.7047117573306,0.));
#9991=CARTESIAN_POINT('Ctrl Pts',(-12.4453471106188,-10.8193387993863,0.));
#9992=CARTESIAN_POINT('Ctrl Pts',(-12.4887054350301,-10.9159571406243,0.));
#9993=CARTESIAN_POINT('Ctrl Pts',(-12.5420886163255,-11.0025423202231,0.));
#9994=CARTESIAN_POINT('Ctrl Pts',(-12.5901836766158,-11.0652195671547,0.));
#9995=CARTESIAN_POINT('Ctrl Pts',(-12.6276288804813,-11.1088271697991,0.));
#9996=CARTESIAN_POINT('Ctrl Pts',(-12.6515210644081,-11.1352828524077,0.));
#9997=CARTESIAN_POINT('Ctrl Pts',(-12.6790250171322,-11.1639734745885,0.));
#9998=CARTESIAN_POINT('Ctrl Pts',(-12.7212344815888,-11.2075126722099,0.));
#9999=CARTESIAN_POINT('Ctrl Pts',(-12.7805989445416,-11.2732934467515,0.));
#10000=CARTESIAN_POINT('Ctrl Pts',(-12.8579347093876,-11.3652836809863,
0.));
#10001=CARTESIAN_POINT('Ctrl Pts',(-12.9451853450404,-11.4773649257318,
0.));
#10002=CARTESIAN_POINT('Ctrl Pts',(-13.0410085154727,-11.6103189008825,
0.));
#10003=CARTESIAN_POINT('Ctrl Pts',(-13.1439278991698,-11.764937382884,0.));
#10004=CARTESIAN_POINT('Ctrl Pts',(-13.2524512620508,-11.9419026340297,
0.));
#10005=CARTESIAN_POINT('Ctrl Pts',(-13.3650363045724,-12.1418243205134,
0.));
#10006=CARTESIAN_POINT('Ctrl Pts',(-13.4801075753502,-12.3652241842034,
0.));
#10007=CARTESIAN_POINT('Ctrl Pts',(-13.6262277632565,-12.6769008431476,
0.));
#10008=CARTESIAN_POINT('Ctrl Pts',(-13.7246099871303,-12.9181650995967,
0.));
#10009=CARTESIAN_POINT('Ctrl Pts',(-13.7839294091566,-13.07682262797,0.));
#10010=CARTESIAN_POINT('',(-13.7360532384392,-8.68235805704666,0.));
#10011=CARTESIAN_POINT('Origin',(0.,0.,0.));
#10012=CARTESIAN_POINT('',(-16.6962658094609,-9.06833546026103,0.));
#10013=CARTESIAN_POINT('Ctrl Pts',(-16.6962658094609,-9.06833546026103,
0.));
#10014=CARTESIAN_POINT('Ctrl Pts',(-16.5270428237395,-9.06094720995301,
0.));
#10015=CARTESIAN_POINT('Ctrl Pts',(-16.2671851013731,-9.0419349102283,0.));
#10016=CARTESIAN_POINT('Ctrl Pts',(-15.9256093626227,-8.99927973772149,
0.));
#10017=CARTESIAN_POINT('Ctrl Pts',(-15.6775844882862,-8.95887481023114,
0.));
#10018=CARTESIAN_POINT('Ctrl Pts',(-15.4526569741556,-8.91357927057118,
0.));
#10019=CARTESIAN_POINT('Ctrl Pts',(-15.2508174554788,-8.8650526891508,0.));
#10020=CARTESIAN_POINT('Ctrl Pts',(-15.0719627020186,-8.81495027721558,
0.));
#10021=CARTESIAN_POINT('Ctrl Pts',(-14.9159049694657,-8.76490206435507,
0.));
#10022=CARTESIAN_POINT('Ctrl Pts',(-14.7823474421093,-8.71655678814369,
0.));
#10023=CARTESIAN_POINT('Ctrl Pts',(-14.6709614647944,-8.67143265073926,
0.));
#10024=CARTESIAN_POINT('Ctrl Pts',(-14.5900556026053,-8.63530106864816,
0.));
#10025=CARTESIAN_POINT('Ctrl Pts',(-14.5356039231527,-8.60861183441385,
0.));
#10026=CARTESIAN_POINT('Ctrl Pts',(-14.4998183311667,-8.59131991078476,
0.));
#10027=CARTESIAN_POINT('Ctrl Pts',(-14.4672743909627,-8.57677234909656,
0.));
#10028=CARTESIAN_POINT('Ctrl Pts',(-14.4142298919554,-8.5546353342573,0.));
#10029=CARTESIAN_POINT('Ctrl Pts',(-14.3397580968625,-8.52826254822913,
0.));
#10030=CARTESIAN_POINT('Ctrl Pts',(-14.2409143873564,-8.50424841775454,
0.));
#10031=CARTESIAN_POINT('Ctrl Pts',(-14.1356264252376,-8.4928689101984,0.));
#10032=CARTESIAN_POINT('Ctrl Pts',(-14.0177193038531,-8.50092900394916,
0.));
#10033=CARTESIAN_POINT('Ctrl Pts',(-13.8694768008521,-8.54836196063206,
0.));
#10034=CARTESIAN_POINT('Ctrl Pts',(-13.7778907925313,-8.62589941321478,
0.));
#10035=CARTESIAN_POINT('Ctrl Pts',(-13.7360532384392,-8.68235805704666,
0.));
#10036=CARTESIAN_POINT('',(-17.1502563092004,-8.1773289360728,0.));
#10037=CARTESIAN_POINT('Origin',(0.,0.,0.));
#10038=CARTESIAN_POINT('',(-15.0980247376579,-6.00933848448149,0.));
#10039=CARTESIAN_POINT('Ctrl Pts',(-15.0980247376579,-6.00933848448149,
0.));
#10040=CARTESIAN_POINT('Ctrl Pts',(-15.0769402326058,-6.07637133495397,
0.));
#10041=CARTESIAN_POINT('Ctrl Pts',(-15.0680440207731,-6.19604134326091,
0.));
#10042=CARTESIAN_POINT('Ctrl Pts',(-15.1168047097502,-6.34385243988823,
0.));
#10043=CARTESIAN_POINT('Ctrl Pts',(-15.1795880240196,-6.44397890908498,
0.));
#10044=CARTESIAN_POINT('Ctrl Pts',(-15.2506809503975,-6.52246995302231,
0.));
#10045=CARTESIAN_POINT('Ctrl Pts',(-15.3282076647862,-6.58832104206025,
0.));
#10046=CARTESIAN_POINT('Ctrl Pts',(-15.3933171197393,-6.63306845520279,
0.));
#10047=CARTESIAN_POINT('Ctrl Pts',(-15.4424051151807,-6.66297054550545,
0.));
#10048=CARTESIAN_POINT('Ctrl Pts',(-15.4733031879166,-6.68074830397729,
0.));
#10049=CARTESIAN_POINT('Ctrl Pts',(-15.5083268912119,-6.69953551835472,
0.));
#10050=CARTESIAN_POINT('Ctrl Pts',(-15.5619248294191,-6.72790031412626,
0.));
#10051=CARTESIAN_POINT('Ctrl Pts',(-15.6387111659832,-6.77211692048665,
0.));
#10052=CARTESIAN_POINT('Ctrl Pts',(-15.7406883947778,-6.8357067665807,0.));
#10053=CARTESIAN_POINT('Ctrl Pts',(-15.8583036897433,-6.91534043556372,
0.));
#10054=CARTESIAN_POINT('Ctrl Pts',(-15.9905219781863,-7.01217619187965,
0.));
#10055=CARTESIAN_POINT('Ctrl Pts',(-16.1361838672874,-7.12742326811382,
0.));
#10056=CARTESIAN_POINT('Ctrl Pts',(-16.2940809887434,-7.26219165995681,
0.));
#10057=CARTESIAN_POINT('Ctrl Pts',(-16.4629349257385,-7.41753779118423,
0.));
#10058=CARTESIAN_POINT('Ctrl Pts',(-16.6414085620714,-7.59444470905136,
0.));
#10059=CARTESIAN_POINT('Ctrl Pts',(-16.8766905033058,-7.84571320523309,
0.));
#10060=CARTESIAN_POINT('Ctrl Pts',(-17.0448123137865,-8.04476736935674,
0.));
#10061=CARTESIAN_POINT('Ctrl Pts',(-17.1502563092004,-8.1773289360728,0.));
#10062=CARTESIAN_POINT('',(-15.7467591314705,-4.0127393206452,0.));
#10063=CARTESIAN_POINT('Origin',(0.,0.,0.));
#10064=CARTESIAN_POINT('',(-18.6813621637974,-3.46506965370684,0.));
#10065=CARTESIAN_POINT('Ctrl Pts',(-18.6813621637974,-3.46506965370684,
0.));
#10066=CARTESIAN_POINT('Ctrl Pts',(-18.5181384456162,-3.51033578853419,
0.));
#10067=CARTESIAN_POINT('Ctrl Pts',(-18.265123941733,-3.57255446932203,0.));
#10068=CARTESIAN_POINT('Ctrl Pts',(-17.9270849363835,-3.63753969769578,
0.));
#10069=CARTESIAN_POINT('Ctrl Pts',(-17.6787134541915,-3.67575622931333,
0.));
#10070=CARTESIAN_POINT('Ctrl Pts',(-17.4507975846592,-3.70218403552949,
0.));
#10071=CARTESIAN_POINT('Ctrl Pts',(-17.2438412568379,-3.71840435546371,
0.));
#10072=CARTESIAN_POINT('Ctrl Pts',(-17.0582577813421,-3.72602328845455,
0.));
#10073=CARTESIAN_POINT('Ctrl Pts',(-16.8943723095674,-3.7266491009471,0.));
#10074=CARTESIAN_POINT('Ctrl Pts',(-16.7524120409277,-3.72194155665402,
0.));
#10075=CARTESIAN_POINT('Ctrl Pts',(-16.632533556064,-3.7134461116587,0.));
#10076=CARTESIAN_POINT('Ctrl Pts',(-16.5444222357228,-3.70408422142789,
0.));
#10077=CARTESIAN_POINT('Ctrl Pts',(-16.4843881842109,-3.69552774561754,
0.));
#10078=CARTESIAN_POINT('Ctrl Pts',(-16.4450105654964,-3.69014050504824,
0.));
#10079=CARTESIAN_POINT('Ctrl Pts',(-16.409563995311,-3.68636158229544,0.));
#10080=CARTESIAN_POINT('Ctrl Pts',(-16.3522749650865,-3.68169968173258,
0.));
#10081=CARTESIAN_POINT('Ctrl Pts',(-16.2732984400115,-3.67963072201294,
0.));
#10082=CARTESIAN_POINT('Ctrl Pts',(-16.1718717115691,-3.68733631276639,
0.));
#10083=CARTESIAN_POINT('Ctrl Pts',(-16.0682204478862,-3.70904952755068,
0.));
#10084=CARTESIAN_POINT('Ctrl Pts',(-15.958574817721,-3.75315043649995,0.));
#10085=CARTESIAN_POINT('Ctrl Pts',(-15.8322454089585,-3.84407131175635,
0.));
#10086=CARTESIAN_POINT('Ctrl Pts',(-15.7691023294921,-3.94611544431017,
0.));
#10087=CARTESIAN_POINT('Ctrl Pts',(-15.7467591314705,-4.0127393206452,0.));
#10088=CARTESIAN_POINT('',(-18.8377966288376,-2.47738131311187,0.));
#10089=CARTESIAN_POINT('Origin',(0.,0.,0.));
#10090=CARTESIAN_POINT('Ctrl Pts',(-16.2160625265912,-1.04967429885971,
0.));
#10091=CARTESIAN_POINT('Ctrl Pts',(-16.2167242606459,-1.11994179848649,
0.));
#10092=CARTESIAN_POINT('Ctrl Pts',(-16.2452435266959,-1.23650382033376,
0.));
#10093=CARTESIAN_POINT('Ctrl Pts',(-16.3372938385016,-1.36201264541056,
0.));
#10094=CARTESIAN_POINT('Ctrl Pts',(-16.4279450992208,-1.43783746532131,
0.));
#10095=CARTESIAN_POINT('Ctrl Pts',(-16.5198135565978,-1.49051796169811,
0.));
#10096=CARTESIAN_POINT('Ctrl Pts',(-16.6138949491149,-1.52918899676863,
0.));
#10097=CARTESIAN_POINT('Ctrl Pts',(-16.6896454316359,-1.55162638755017,
0.));
#10098=CARTESIAN_POINT('Ctrl Pts',(-16.7455711436431,-1.56489594057219,
0.));
#10099=CARTESIAN_POINT('Ctrl Pts',(-16.7804505865492,-1.57225556404312,
0.));
#10100=CARTESIAN_POINT('Ctrl Pts',(-16.8195656763126,-1.57930034717562,
0.));
#10101=CARTESIAN_POINT('Ctrl Pts',(-16.8793055486399,-1.58971419725805,
0.));
#10102=CARTESIAN_POINT('Ctrl Pts',(-16.9659973771906,-1.60803840593145,
0.));
#10103=CARTESIAN_POINT('Ctrl Pts',(-17.0826338282621,-1.63700324669261,
0.));
#10104=CARTESIAN_POINT('Ctrl Pts',(-17.2191007779953,-1.67639424155264,
0.));
#10105=CARTESIAN_POINT('Ctrl Pts',(-17.3747717371572,-1.72763282051121,
0.));
#10106=CARTESIAN_POINT('Ctrl Pts',(-17.548917731071,-1.79222730418269,0.));
#10107=CARTESIAN_POINT('Ctrl Pts',(-17.7407325407201,-1.87160676754278,
0.));
#10108=CARTESIAN_POINT('Ctrl Pts',(-17.949326772361,-1.96717098182925,0.));
#10109=CARTESIAN_POINT('Ctrl Pts',(-18.1737325312258,-2.08026807216972,
0.));
#10110=CARTESIAN_POINT('Ctrl Pts',(-18.4751451900744,-2.2465324944921,0.));
#10111=CARTESIAN_POINT('Ctrl Pts',(-18.6965496529788,-2.38389175781394,
0.));
#10112=CARTESIAN_POINT('Ctrl Pts',(-18.8377966288376,-2.47738131311187,
0.));
#10113=CARTESIAN_POINT('',(-18.8377966288375,2.47738131311205,0.));
#10114=CARTESIAN_POINT('Ctrl Pts',(-18.8377966288375,2.47738131311205,0.));
#10115=CARTESIAN_POINT('Ctrl Pts',(-18.6965496529788,2.38389175781397,0.));
#10116=CARTESIAN_POINT('Ctrl Pts',(-18.4751451900744,2.24653249449212,0.));
#10117=CARTESIAN_POINT('Ctrl Pts',(-18.1737325312257,2.08026807216975,0.));
#10118=CARTESIAN_POINT('Ctrl Pts',(-17.949326772361,1.96717098182926,0.));
#10119=CARTESIAN_POINT('Ctrl Pts',(-17.7407325407201,1.87160676754277,0.));
#10120=CARTESIAN_POINT('Ctrl Pts',(-17.548917731071,1.79222730418272,0.));
#10121=CARTESIAN_POINT('Ctrl Pts',(-17.3747717371572,1.72763282051119,0.));
#10122=CARTESIAN_POINT('Ctrl Pts',(-17.2191007779952,1.67639424155264,0.));
#10123=CARTESIAN_POINT('Ctrl Pts',(-17.0826338282621,1.63700324669263,0.));
#10124=CARTESIAN_POINT('Ctrl Pts',(-16.9659973771906,1.60803840593145,0.));
#10125=CARTESIAN_POINT('Ctrl Pts',(-16.8793055486399,1.58971419725805,0.));
#10126=CARTESIAN_POINT('Ctrl Pts',(-16.8195656763126,1.57930034717566,0.));
#10127=CARTESIAN_POINT('Ctrl Pts',(-16.7804505865492,1.57225556404312,0.));
#10128=CARTESIAN_POINT('Ctrl Pts',(-16.7455711436431,1.56489594057218,0.));
#10129=CARTESIAN_POINT('Ctrl Pts',(-16.6896454316358,1.55162638755017,0.));
#10130=CARTESIAN_POINT('Ctrl Pts',(-16.6138949491149,1.52918899676863,0.));
#10131=CARTESIAN_POINT('Ctrl Pts',(-16.5198135565977,1.4905179616981,0.));
#10132=CARTESIAN_POINT('Ctrl Pts',(-16.4279450992207,1.43783746532133,0.));
#10133=CARTESIAN_POINT('Ctrl Pts',(-16.3372938385016,1.3620126454106,0.));
#10134=CARTESIAN_POINT('Ctrl Pts',(-16.2452435266959,1.23650382033378,0.));
#10135=CARTESIAN_POINT('Ctrl Pts',(-16.2167242606458,1.1199417984865,0.));
#10136=CARTESIAN_POINT('Ctrl Pts',(-16.2160625265911,1.04967429885986,0.));
#10137=CARTESIAN_POINT('',(-18.6813621637973,3.46506965370702,0.));
#10138=CARTESIAN_POINT('Origin',(0.,0.,0.));
#10139=CARTESIAN_POINT('',(-15.7467591314704,4.01273932064536,0.));
#10140=CARTESIAN_POINT('Ctrl Pts',(-15.7467591314704,4.01273932064536,0.));
#10141=CARTESIAN_POINT('Ctrl Pts',(-15.7691023294921,3.94611544431018,0.));
#10142=CARTESIAN_POINT('Ctrl Pts',(-15.8322454089585,3.84407131175636,0.));
#10143=CARTESIAN_POINT('Ctrl Pts',(-15.958574817721,3.75315043649999,0.));
#10144=CARTESIAN_POINT('Ctrl Pts',(-16.0682204478862,3.7090495275507,0.));
#10145=CARTESIAN_POINT('Ctrl Pts',(-16.1718717115691,3.68733631276638,0.));
#10146=CARTESIAN_POINT('Ctrl Pts',(-16.2732984400115,3.67963072201295,0.));
#10147=CARTESIAN_POINT('Ctrl Pts',(-16.3522749650865,3.68169968173258,0.));
#10148=CARTESIAN_POINT('Ctrl Pts',(-16.409563995311,3.68636158229543,0.));
#10149=CARTESIAN_POINT('Ctrl Pts',(-16.4450105654964,3.69014050504823,0.));
#10150=CARTESIAN_POINT('Ctrl Pts',(-16.4843881842109,3.69552774561757,0.));
#10151=CARTESIAN_POINT('Ctrl Pts',(-16.5444222357228,3.70408422142789,0.));
#10152=CARTESIAN_POINT('Ctrl Pts',(-16.632533556064,3.7134461116587,0.));
#10153=CARTESIAN_POINT('Ctrl Pts',(-16.7524120409277,3.72194155665404,0.));
#10154=CARTESIAN_POINT('Ctrl Pts',(-16.8943723095674,3.72664910094711,0.));
#10155=CARTESIAN_POINT('Ctrl Pts',(-17.0582577813421,3.72602328845453,0.));
#10156=CARTESIAN_POINT('Ctrl Pts',(-17.2438412568379,3.71840435546374,0.));
#10157=CARTESIAN_POINT('Ctrl Pts',(-17.4507975846592,3.70218403552947,0.));
#10158=CARTESIAN_POINT('Ctrl Pts',(-17.6787134541915,3.67575622931334,0.));
#10159=CARTESIAN_POINT('Ctrl Pts',(-17.9270849363835,3.63753969769581,0.));
#10160=CARTESIAN_POINT('Ctrl Pts',(-18.265123941733,3.57255446932205,0.));
#10161=CARTESIAN_POINT('Ctrl Pts',(-18.5181384456163,3.51033578853423,0.));
#10162=CARTESIAN_POINT('Ctrl Pts',(-18.6813621637973,3.46506965370702,0.));
#10163=CARTESIAN_POINT('',(-15.0980247376578,6.00933848448163,0.));
#10164=CARTESIAN_POINT('Origin',(0.,0.,0.));
#10165=CARTESIAN_POINT('',(-17.1502563092003,8.17732893607296,0.));
#10166=CARTESIAN_POINT('Ctrl Pts',(-17.1502563092003,8.17732893607296,0.));
#10167=CARTESIAN_POINT('Ctrl Pts',(-17.0448123137865,8.04476736935675,0.));
#10168=CARTESIAN_POINT('Ctrl Pts',(-16.8766905033057,7.8457132052331,0.));
#10169=CARTESIAN_POINT('Ctrl Pts',(-16.6414085620714,7.59444470905138,0.));
#10170=CARTESIAN_POINT('Ctrl Pts',(-16.4629349257385,7.41753779118423,0.));
#10171=CARTESIAN_POINT('Ctrl Pts',(-16.2940809887434,7.26219165995682,0.));
#10172=CARTESIAN_POINT('Ctrl Pts',(-16.1361838672874,7.12742326811386,0.));
#10173=CARTESIAN_POINT('Ctrl Pts',(-15.9905219781863,7.01217619187965,0.));
#10174=CARTESIAN_POINT('Ctrl Pts',(-15.8583036897432,6.91534043556372,0.));
#10175=CARTESIAN_POINT('Ctrl Pts',(-15.7406883947777,6.83570676658073,0.));
#10176=CARTESIAN_POINT('Ctrl Pts',(-15.6387111659832,6.77211692048666,0.));
#10177=CARTESIAN_POINT('Ctrl Pts',(-15.5619248294191,6.72790031412627,0.));
#10178=CARTESIAN_POINT('Ctrl Pts',(-15.5083268912118,6.69953551835476,0.));
#10179=CARTESIAN_POINT('Ctrl Pts',(-15.4733031879166,6.68074830397729,0.));
#10180=CARTESIAN_POINT('Ctrl Pts',(-15.4424051151807,6.66297054550545,0.));
#10181=CARTESIAN_POINT('Ctrl Pts',(-15.3933171197393,6.6330684552028,0.));
#10182=CARTESIAN_POINT('Ctrl Pts',(-15.3282076647861,6.58832104206026,0.));
#10183=CARTESIAN_POINT('Ctrl Pts',(-15.2506809503975,6.5224699530223,0.));
#10184=CARTESIAN_POINT('Ctrl Pts',(-15.1795880240196,6.443978909085,0.));
#10185=CARTESIAN_POINT('Ctrl Pts',(-15.1168047097501,6.34385243988827,0.));
#10186=CARTESIAN_POINT('Ctrl Pts',(-15.0680440207731,6.19604134326095,0.));
#10187=CARTESIAN_POINT('Ctrl Pts',(-15.0769402326058,6.07637133495398,0.));
#10188=CARTESIAN_POINT('Ctrl Pts',(-15.0980247376578,6.00933848448163,0.));
#10189=CARTESIAN_POINT('',(-16.6962658094608,9.06833546026117,0.));
#10190=CARTESIAN_POINT('Origin',(-1.73472347597681E-15,0.,0.));
#10191=CARTESIAN_POINT('',(-13.7360532384391,8.68235805704682,0.));
#10192=CARTESIAN_POINT('Ctrl Pts',(-13.7360532384391,8.68235805704682,0.));
#10193=CARTESIAN_POINT('Ctrl Pts',(-13.7778907925313,8.62589941321479,0.));
#10194=CARTESIAN_POINT('Ctrl Pts',(-13.8694768008521,8.54836196063206,0.));
#10195=CARTESIAN_POINT('Ctrl Pts',(-14.0177193038531,8.50092900394919,0.));
#10196=CARTESIAN_POINT('Ctrl Pts',(-14.1356264252377,8.49286891019842,0.));
#10197=CARTESIAN_POINT('Ctrl Pts',(-14.2409143873564,8.50424841775455,0.));
#10198=CARTESIAN_POINT('Ctrl Pts',(-14.3397580968626,8.52826254822914,0.));
#10199=CARTESIAN_POINT('Ctrl Pts',(-14.4142298919555,8.55463533425731,0.));
#10200=CARTESIAN_POINT('Ctrl Pts',(-14.4672743909627,8.57677234909655,0.));
#10201=CARTESIAN_POINT('Ctrl Pts',(-14.4998183311667,8.59131991078475,0.));
#10202=CARTESIAN_POINT('Ctrl Pts',(-14.5356039231527,8.60861183441388,0.));
#10203=CARTESIAN_POINT('Ctrl Pts',(-14.5900556026053,8.63530106864817,0.));
#10204=CARTESIAN_POINT('Ctrl Pts',(-14.6709614647944,8.67143265073926,0.));
#10205=CARTESIAN_POINT('Ctrl Pts',(-14.7823474421093,8.71655678814371,0.));
#10206=CARTESIAN_POINT('Ctrl Pts',(-14.9159049694657,8.76490206435508,0.));
#10207=CARTESIAN_POINT('Ctrl Pts',(-15.0719627020186,8.81495027721556,0.));
#10208=CARTESIAN_POINT('Ctrl Pts',(-15.2508174554788,8.86505268915083,0.));
#10209=CARTESIAN_POINT('Ctrl Pts',(-15.4526569741556,8.91357927057117,0.));
#10210=CARTESIAN_POINT('Ctrl Pts',(-15.6775844882863,8.95887481023116,0.));
#10211=CARTESIAN_POINT('Ctrl Pts',(-15.9256093626227,8.99927973772153,0.));
#10212=CARTESIAN_POINT('Ctrl Pts',(-16.2671851013731,9.04193491022832,0.));
#10213=CARTESIAN_POINT('Ctrl Pts',(-16.5270428237395,9.06094720995306,0.));
#10214=CARTESIAN_POINT('Ctrl Pts',(-16.6962658094608,9.06833546026117,0.));
#10215=CARTESIAN_POINT('',(-12.5020870932787,10.3807667497191,0.));
#10216=CARTESIAN_POINT('Origin',(0.,0.,0.));
#10217=CARTESIAN_POINT('',(-13.7839294091564,13.0768226279702,0.));
#10218=CARTESIAN_POINT('Ctrl Pts',(-13.7839294091564,13.0768226279702,0.));
#10219=CARTESIAN_POINT('Ctrl Pts',(-13.7246099871302,12.9181650995968,0.));
#10220=CARTESIAN_POINT('Ctrl Pts',(-13.6262277632565,12.6769008431476,0.));
#10221=CARTESIAN_POINT('Ctrl Pts',(-13.4801075753502,12.3652241842034,0.));
#10222=CARTESIAN_POINT('Ctrl Pts',(-13.3650363045723,12.1418243205134,0.));
#10223=CARTESIAN_POINT('Ctrl Pts',(-13.2524512620508,11.9419026340297,0.));
#10224=CARTESIAN_POINT('Ctrl Pts',(-13.1439278991698,11.764937382884,0.));
#10225=CARTESIAN_POINT('Ctrl Pts',(-13.0410085154728,11.6103189008826,0.));
#10226=CARTESIAN_POINT('Ctrl Pts',(-12.9451853450404,11.4773649257318,0.));
#10227=CARTESIAN_POINT('Ctrl Pts',(-12.8579347093876,11.3652836809863,0.));
#10228=CARTESIAN_POINT('Ctrl Pts',(-12.7805989445416,11.2732934467516,0.));
#10229=CARTESIAN_POINT('Ctrl Pts',(-12.7212344815888,11.2075126722099,0.));
#10230=CARTESIAN_POINT('Ctrl Pts',(-12.6790250171322,11.1639734745886,0.));
#10231=CARTESIAN_POINT('Ctrl Pts',(-12.651521064408,11.1352828524077,0.));
#10232=CARTESIAN_POINT('Ctrl Pts',(-12.6276288804813,11.1088271697991,0.));
#10233=CARTESIAN_POINT('Ctrl Pts',(-12.5901836766158,11.0652195671547,0.));
#10234=CARTESIAN_POINT('Ctrl Pts',(-12.5420886163255,11.0025423202231,0.));
#10235=CARTESIAN_POINT('Ctrl Pts',(-12.48870543503,10.9159571406243,0.));
#10236=CARTESIAN_POINT('Ctrl Pts',(-12.4453471106187,10.8193387993863,0.));
#10237=CARTESIAN_POINT('Ctrl Pts',(-12.4165774110367,10.7047117573307,0.));
#10238=CARTESIAN_POINT('Ctrl Pts',(-12.4158793808611,10.5490671691512,0.));
#10239=CARTESIAN_POINT('Ctrl Pts',(-12.4613202473787,10.4380033085876,0.));
#10240=CARTESIAN_POINT('Ctrl Pts',(-12.5020870932787,10.3807667497191,0.));
#10241=CARTESIAN_POINT('',(-13.07682262797,13.7839294091566,0.));
#10242=CARTESIAN_POINT('Origin',(1.57723797680727E-16,0.,0.));
#10243=CARTESIAN_POINT('',(-10.380766749719,12.5020870932788,0.));
#10244=CARTESIAN_POINT('Ctrl Pts',(-10.380766749719,12.5020870932788,0.));
#10245=CARTESIAN_POINT('Ctrl Pts',(-10.4380033085876,12.4613202473787,0.));
#10246=CARTESIAN_POINT('Ctrl Pts',(-10.5490671691512,12.4158793808611,0.));
#10247=CARTESIAN_POINT('Ctrl Pts',(-10.7047117573307,12.4165774110367,0.));
#10248=CARTESIAN_POINT('Ctrl Pts',(-10.8193387993863,12.4453471106187,0.));
#10249=CARTESIAN_POINT('Ctrl Pts',(-10.9159571406243,12.48870543503,0.));
#10250=CARTESIAN_POINT('Ctrl Pts',(-11.0025423202232,12.5420886163255,0.));
#10251=CARTESIAN_POINT('Ctrl Pts',(-11.0652195671547,12.5901836766158,0.));
#10252=CARTESIAN_POINT('Ctrl Pts',(-11.1088271697991,12.6276288804813,0.));
#10253=CARTESIAN_POINT('Ctrl Pts',(-11.1352828524077,12.651521064408,0.));
#10254=CARTESIAN_POINT('Ctrl Pts',(-11.1639734745886,12.6790250171322,0.));
#10255=CARTESIAN_POINT('Ctrl Pts',(-11.20751267221,12.7212344815888,0.));
#10256=CARTESIAN_POINT('Ctrl Pts',(-11.2732934467516,12.7805989445416,0.));
#10257=CARTESIAN_POINT('Ctrl Pts',(-11.3652836809863,12.8579347093876,0.));
#10258=CARTESIAN_POINT('Ctrl Pts',(-11.4773649257319,12.9451853450404,0.));
#10259=CARTESIAN_POINT('Ctrl Pts',(-11.6103189008826,13.0410085154727,0.));
#10260=CARTESIAN_POINT('Ctrl Pts',(-11.764937382884,13.1439278991698,0.));
#10261=CARTESIAN_POINT('Ctrl Pts',(-11.9419026340297,13.2524512620507,0.));
#10262=CARTESIAN_POINT('Ctrl Pts',(-12.1418243205134,13.3650363045724,0.));
#10263=CARTESIAN_POINT('Ctrl Pts',(-12.3652241842034,13.4801075753502,0.));
#10264=CARTESIAN_POINT('Ctrl Pts',(-12.6769008431476,13.6262277632565,0.));
#10265=CARTESIAN_POINT('Ctrl Pts',(-12.9181650995968,13.7246099871303,0.));
#10266=CARTESIAN_POINT('Ctrl Pts',(-13.07682262797,13.7839294091566,0.));
#10267=CARTESIAN_POINT('',(-8.68235805704666,13.7360532384392,0.));
#10268=CARTESIAN_POINT('Origin',(0.,0.,0.));
#10269=CARTESIAN_POINT('',(-9.06833546026097,16.6962658094609,0.));
#10270=CARTESIAN_POINT('Ctrl Pts',(-9.06833546026097,16.6962658094609,0.));
#10271=CARTESIAN_POINT('Ctrl Pts',(-9.06094720995302,16.5270428237395,0.));
#10272=CARTESIAN_POINT('Ctrl Pts',(-9.04193491022831,16.2671851013731,0.));
#10273=CARTESIAN_POINT('Ctrl Pts',(-8.9992797377215,15.9256093626227,0.));
#10274=CARTESIAN_POINT('Ctrl Pts',(-8.95887481023115,15.6775844882862,0.));
#10275=CARTESIAN_POINT('Ctrl Pts',(-8.91357927057119,15.4526569741556,0.));
#10276=CARTESIAN_POINT('Ctrl Pts',(-8.8650526891508,15.2508174554788,0.));
#10277=CARTESIAN_POINT('Ctrl Pts',(-8.81495027721559,15.0719627020186,0.));
#10278=CARTESIAN_POINT('Ctrl Pts',(-8.76490206435507,14.9159049694657,0.));
#10279=CARTESIAN_POINT('Ctrl Pts',(-8.71655678814369,14.7823474421093,0.));
#10280=CARTESIAN_POINT('Ctrl Pts',(-8.67143265073926,14.6709614647944,0.));
#10281=CARTESIAN_POINT('Ctrl Pts',(-8.63530106864816,14.5900556026053,0.));
#10282=CARTESIAN_POINT('Ctrl Pts',(-8.60861183441386,14.5356039231527,0.));
#10283=CARTESIAN_POINT('Ctrl Pts',(-8.59131991078476,14.4998183311667,0.));
#10284=CARTESIAN_POINT('Ctrl Pts',(-8.57677234909655,14.4672743909627,0.));
#10285=CARTESIAN_POINT('Ctrl Pts',(-8.55463533425729,14.4142298919554,0.));
#10286=CARTESIAN_POINT('Ctrl Pts',(-8.52826254822913,14.3397580968626,0.));
#10287=CARTESIAN_POINT('Ctrl Pts',(-8.50424841775454,14.2409143873564,0.));
#10288=CARTESIAN_POINT('Ctrl Pts',(-8.49286891019839,14.1356264252377,0.));
#10289=CARTESIAN_POINT('Ctrl Pts',(-8.50092900394916,14.0177193038531,0.));
#10290=CARTESIAN_POINT('Ctrl Pts',(-8.54836196063204,13.8694768008521,0.));
#10291=CARTESIAN_POINT('Ctrl Pts',(-8.62589941321477,13.7778907925313,0.));
#10292=CARTESIAN_POINT('Ctrl Pts',(-8.68235805704666,13.7360532384392,0.));
#10293=CARTESIAN_POINT('',(-8.1773289360728,17.1502563092004,0.));
#10294=CARTESIAN_POINT('Origin',(1.73472347597681E-15,0.,0.));
#10295=CARTESIAN_POINT('',(-6.00933848448141,15.0980247376579,0.));
#10296=CARTESIAN_POINT('Ctrl Pts',(-6.00933848448141,15.0980247376579,0.));
#10297=CARTESIAN_POINT('Ctrl Pts',(-6.076371334954,15.0769402326058,0.));
#10298=CARTESIAN_POINT('Ctrl Pts',(-6.19604134326094,15.0680440207731,0.));
#10299=CARTESIAN_POINT('Ctrl Pts',(-6.34385243988825,15.1168047097501,0.));
#10300=CARTESIAN_POINT('Ctrl Pts',(-6.44397890908501,15.1795880240196,0.));
#10301=CARTESIAN_POINT('Ctrl Pts',(-6.52246995302233,15.2506809503975,0.));
#10302=CARTESIAN_POINT('Ctrl Pts',(-6.58832104206028,15.3282076647862,0.));
#10303=CARTESIAN_POINT('Ctrl Pts',(-6.63306845520281,15.3933171197393,0.));
#10304=CARTESIAN_POINT('Ctrl Pts',(-6.66297054550547,15.4424051151807,0.));
#10305=CARTESIAN_POINT('Ctrl Pts',(-6.68074830397731,15.4733031879166,0.));
#10306=CARTESIAN_POINT('Ctrl Pts',(-6.69953551835474,15.5083268912119,0.));
#10307=CARTESIAN_POINT('Ctrl Pts',(-6.72790031412628,15.5619248294191,0.));
#10308=CARTESIAN_POINT('Ctrl Pts',(-6.77211692048667,15.6387111659832,0.));
#10309=CARTESIAN_POINT('Ctrl Pts',(-6.83570676658072,15.7406883947778,0.));
#10310=CARTESIAN_POINT('Ctrl Pts',(-6.91534043556374,15.8583036897433,0.));
#10311=CARTESIAN_POINT('Ctrl Pts',(-7.01217619187967,15.9905219781863,0.));
#10312=CARTESIAN_POINT('Ctrl Pts',(-7.12742326811385,16.1361838672874,0.));
#10313=CARTESIAN_POINT('Ctrl Pts',(-7.26219165995682,16.2940809887434,0.));
#10314=CARTESIAN_POINT('Ctrl Pts',(-7.41753779118424,16.4629349257385,0.));
#10315=CARTESIAN_POINT('Ctrl Pts',(-7.59444470905137,16.6414085620714,0.));
#10316=CARTESIAN_POINT('Ctrl Pts',(-7.8457132052331,16.8766905033058,0.));
#10317=CARTESIAN_POINT('Ctrl Pts',(-8.04476736935674,17.0448123137865,0.));
#10318=CARTESIAN_POINT('Ctrl Pts',(-8.1773289360728,17.1502563092004,0.));
#10319=CARTESIAN_POINT('',(-4.01273932064518,15.7467591314705,0.));
#10320=CARTESIAN_POINT('Origin',(0.,0.,0.));
#10321=CARTESIAN_POINT('',(-3.46506965370679,18.6813621637974,0.));
#10322=CARTESIAN_POINT('Ctrl Pts',(-3.46506965370679,18.6813621637974,0.));
#10323=CARTESIAN_POINT('Ctrl Pts',(-3.51033578853418,18.5181384456162,0.));
#10324=CARTESIAN_POINT('Ctrl Pts',(-3.57255446932203,18.265123941733,0.));
#10325=CARTESIAN_POINT('Ctrl Pts',(-3.63753969769577,17.9270849363835,0.));
#10326=CARTESIAN_POINT('Ctrl Pts',(-3.67575622931332,17.6787134541915,0.));
#10327=CARTESIAN_POINT('Ctrl Pts',(-3.70218403552948,17.4507975846592,0.));
#10328=CARTESIAN_POINT('Ctrl Pts',(-3.7184043554637,17.2438412568379,0.));
#10329=CARTESIAN_POINT('Ctrl Pts',(-3.72602328845454,17.0582577813421,0.));
#10330=CARTESIAN_POINT('Ctrl Pts',(-3.72664910094709,16.8943723095674,0.));
#10331=CARTESIAN_POINT('Ctrl Pts',(-3.72194155665401,16.7524120409277,0.));
#10332=CARTESIAN_POINT('Ctrl Pts',(-3.71344611165868,16.632533556064,0.));
#10333=CARTESIAN_POINT('Ctrl Pts',(-3.70408422142788,16.5444222357228,0.));
#10334=CARTESIAN_POINT('Ctrl Pts',(-3.69552774561753,16.4843881842109,0.));
#10335=CARTESIAN_POINT('Ctrl Pts',(-3.69014050504823,16.4450105654964,0.));
#10336=CARTESIAN_POINT('Ctrl Pts',(-3.68636158229542,16.409563995311,0.));
#10337=CARTESIAN_POINT('Ctrl Pts',(-3.68169968173256,16.3522749650865,0.));
#10338=CARTESIAN_POINT('Ctrl Pts',(-3.67963072201293,16.2732984400115,0.));
#10339=CARTESIAN_POINT('Ctrl Pts',(-3.68733631276638,16.1718717115691,0.));
#10340=CARTESIAN_POINT('Ctrl Pts',(-3.70904952755066,16.0682204478862,0.));
#10341=CARTESIAN_POINT('Ctrl Pts',(-3.75315043649994,15.958574817721,0.));
#10342=CARTESIAN_POINT('Ctrl Pts',(-3.84407131175633,15.8322454089585,0.));
#10343=CARTESIAN_POINT('Ctrl Pts',(-3.94611544431016,15.7691023294921,0.));
#10344=CARTESIAN_POINT('Ctrl Pts',(-4.01273932064518,15.7467591314705,0.));
#10345=CARTESIAN_POINT('',(-2.47738131311187,18.8377966288376,0.));
#10346=CARTESIAN_POINT('Origin',(-1.73472347597681E-15,0.,0.));
#10347=CARTESIAN_POINT('',(-1.04967429885962,16.2160625265911,0.));
#10348=CARTESIAN_POINT('Ctrl Pts',(-1.04967429885962,16.2160625265911,0.));
#10349=CARTESIAN_POINT('Ctrl Pts',(-1.11994179848651,16.2167242606459,0.));
#10350=CARTESIAN_POINT('Ctrl Pts',(-1.23650382033378,16.2452435266959,0.));
#10351=CARTESIAN_POINT('Ctrl Pts',(-1.36201264541058,16.3372938385016,0.));
#10352=CARTESIAN_POINT('Ctrl Pts',(-1.43783746532133,16.4279450992208,0.));
#10353=CARTESIAN_POINT('Ctrl Pts',(-1.49051796169812,16.5198135565978,0.));
#10354=CARTESIAN_POINT('Ctrl Pts',(-1.52918899676864,16.6138949491149,0.));
#10355=CARTESIAN_POINT('Ctrl Pts',(-1.55162638755018,16.6896454316359,0.));
#10356=CARTESIAN_POINT('Ctrl Pts',(-1.5648959405722,16.7455711436431,0.));
#10357=CARTESIAN_POINT('Ctrl Pts',(-1.57225556404314,16.7804505865492,0.));
#10358=CARTESIAN_POINT('Ctrl Pts',(-1.57930034717564,16.8195656763126,0.));
#10359=CARTESIAN_POINT('Ctrl Pts',(-1.58971419725806,16.8793055486399,0.));
#10360=CARTESIAN_POINT('Ctrl Pts',(-1.60803840593146,16.9659973771906,0.));
#10361=CARTESIAN_POINT('Ctrl Pts',(-1.63700324669262,17.0826338282622,0.));
#10362=CARTESIAN_POINT('Ctrl Pts',(-1.67639424155265,17.2191007779953,0.));
#10363=CARTESIAN_POINT('Ctrl Pts',(-1.72763282051122,17.3747717371572,0.));
#10364=CARTESIAN_POINT('Ctrl Pts',(-1.7922273041827,17.548917731071,0.));
#10365=CARTESIAN_POINT('Ctrl Pts',(-1.87160676754278,17.7407325407201,0.));
#10366=CARTESIAN_POINT('Ctrl Pts',(-1.96717098182926,17.949326772361,0.));
#10367=CARTESIAN_POINT('Ctrl Pts',(-2.08026807216973,18.1737325312257,0.));
#10368=CARTESIAN_POINT('Ctrl Pts',(-2.24653249449211,18.4751451900744,0.));
#10369=CARTESIAN_POINT('Ctrl Pts',(-2.38389175781394,18.6965496529788,0.));
#10370=CARTESIAN_POINT('Ctrl Pts',(-2.47738131311187,18.8377966288376,0.));
#10371=CARTESIAN_POINT('',(1.04967429885989,16.2160625265911,0.));
#10372=CARTESIAN_POINT('Origin',(0.,0.,0.));
#10373=CARTESIAN_POINT('',(2.47738131311212,18.8377966288375,0.));
#10374=CARTESIAN_POINT('Ctrl Pts',(2.47738131311212,18.8377966288375,0.));
#10375=CARTESIAN_POINT('Ctrl Pts',(2.38389175781397,18.6965496529788,0.));
#10376=CARTESIAN_POINT('Ctrl Pts',(2.24653249449213,18.4751451900744,0.));
#10377=CARTESIAN_POINT('Ctrl Pts',(2.08026807216976,18.1737325312257,0.));
#10378=CARTESIAN_POINT('Ctrl Pts',(1.96717098182927,17.949326772361,0.));
#10379=CARTESIAN_POINT('Ctrl Pts',(1.87160676754279,17.7407325407201,0.));
#10380=CARTESIAN_POINT('Ctrl Pts',(1.79222730418274,17.548917731071,0.));
#10381=CARTESIAN_POINT('Ctrl Pts',(1.72763282051121,17.3747717371572,0.));
#10382=CARTESIAN_POINT('Ctrl Pts',(1.67639424155266,17.2191007779952,0.));
#10383=CARTESIAN_POINT('Ctrl Pts',(1.63700324669265,17.0826338282621,0.));
#10384=CARTESIAN_POINT('Ctrl Pts',(1.60803840593148,16.9659973771906,0.));
#10385=CARTESIAN_POINT('Ctrl Pts',(1.58971419725808,16.8793055486399,0.));
#10386=CARTESIAN_POINT('Ctrl Pts',(1.57930034717568,16.8195656763126,0.));
#10387=CARTESIAN_POINT('Ctrl Pts',(1.57225556404314,16.7804505865492,0.));
#10388=CARTESIAN_POINT('Ctrl Pts',(1.5648959405722,16.7455711436431,0.));
#10389=CARTESIAN_POINT('Ctrl Pts',(1.5516263875502,16.6896454316358,0.));
#10390=CARTESIAN_POINT('Ctrl Pts',(1.52918899676866,16.6138949491149,0.));
#10391=CARTESIAN_POINT('Ctrl Pts',(1.49051796169813,16.5198135565977,0.));
#10392=CARTESIAN_POINT('Ctrl Pts',(1.43783746532136,16.4279450992207,0.));
#10393=CARTESIAN_POINT('Ctrl Pts',(1.36201264541063,16.3372938385016,0.));
#10394=CARTESIAN_POINT('Ctrl Pts',(1.23650382033381,16.2452435266959,0.));
#10395=CARTESIAN_POINT('Ctrl Pts',(1.11994179848653,16.2167242606458,0.));
#10396=CARTESIAN_POINT('Ctrl Pts',(1.04967429885989,16.2160625265911,0.));
#10397=CARTESIAN_POINT('',(3.46506965370702,18.6813621637974,0.));
#10398=CARTESIAN_POINT('Origin',(0.,8.67361737988404E-16,0.));
#10399=CARTESIAN_POINT('',(4.01273932064543,15.7467591314704,0.));
#10400=CARTESIAN_POINT('Ctrl Pts',(4.01273932064543,15.7467591314704,0.));
#10401=CARTESIAN_POINT('Ctrl Pts',(3.94611544431017,15.7691023294921,0.));
#10402=CARTESIAN_POINT('Ctrl Pts',(3.84407131175635,15.8322454089585,0.));
#10403=CARTESIAN_POINT('Ctrl Pts',(3.75315043649997,15.9585748177211,0.));
#10404=CARTESIAN_POINT('Ctrl Pts',(3.70904952755068,16.0682204478862,0.));
#10405=CARTESIAN_POINT('Ctrl Pts',(3.68733631276637,16.1718717115691,0.));
#10406=CARTESIAN_POINT('Ctrl Pts',(3.67963072201293,16.2732984400116,0.));
#10407=CARTESIAN_POINT('Ctrl Pts',(3.68169968173257,16.3522749650866,0.));
#10408=CARTESIAN_POINT('Ctrl Pts',(3.68636158229542,16.409563995311,0.));
#10409=CARTESIAN_POINT('Ctrl Pts',(3.69014050504822,16.4450105654964,0.));
#10410=CARTESIAN_POINT('Ctrl Pts',(3.69552774561756,16.4843881842109,0.));
#10411=CARTESIAN_POINT('Ctrl Pts',(3.70408422142788,16.5444222357228,0.));
#10412=CARTESIAN_POINT('Ctrl Pts',(3.71344611165869,16.632533556064,0.));
#10413=CARTESIAN_POINT('Ctrl Pts',(3.72194155665403,16.7524120409277,0.));
#10414=CARTESIAN_POINT('Ctrl Pts',(3.7266491009471,16.8943723095674,0.));
#10415=CARTESIAN_POINT('Ctrl Pts',(3.72602328845452,17.0582577813421,0.));
#10416=CARTESIAN_POINT('Ctrl Pts',(3.71840435546373,17.2438412568379,0.));
#10417=CARTESIAN_POINT('Ctrl Pts',(3.70218403552947,17.4507975846592,0.));
#10418=CARTESIAN_POINT('Ctrl Pts',(3.67575622931333,17.6787134541915,0.));
#10419=CARTESIAN_POINT('Ctrl Pts',(3.63753969769581,17.9270849363835,0.));
#10420=CARTESIAN_POINT('Ctrl Pts',(3.57255446932205,18.265123941733,0.));
#10421=CARTESIAN_POINT('Ctrl Pts',(3.51033578853423,18.5181384456163,0.));
#10422=CARTESIAN_POINT('Ctrl Pts',(3.46506965370702,18.6813621637974,0.));
#10423=CARTESIAN_POINT('',(6.00933848448158,15.0980247376579,0.));
#10424=CARTESIAN_POINT('Origin',(0.,0.,0.));
#10425=CARTESIAN_POINT('',(8.17732893607301,17.1502563092002,0.));
#10426=CARTESIAN_POINT('Ctrl Pts',(8.17732893607301,17.1502563092002,0.));
#10427=CARTESIAN_POINT('Ctrl Pts',(8.04476736935673,17.0448123137865,0.));
#10428=CARTESIAN_POINT('Ctrl Pts',(7.84571320523309,16.8766905033057,0.));
#10429=CARTESIAN_POINT('Ctrl Pts',(7.59444470905135,16.6414085620714,0.));
#10430=CARTESIAN_POINT('Ctrl Pts',(7.4175377911842,16.4629349257385,0.));
#10431=CARTESIAN_POINT('Ctrl Pts',(7.26219165995678,16.2940809887434,0.));
#10432=CARTESIAN_POINT('Ctrl Pts',(7.12742326811382,16.1361838672874,0.));
#10433=CARTESIAN_POINT('Ctrl Pts',(7.01217619187961,15.9905219781863,0.));
#10434=CARTESIAN_POINT('Ctrl Pts',(6.91534043556368,15.8583036897433,0.));
#10435=CARTESIAN_POINT('Ctrl Pts',(6.83570676658068,15.7406883947777,0.));
#10436=CARTESIAN_POINT('Ctrl Pts',(6.77211692048662,15.6387111659832,0.));
#10437=CARTESIAN_POINT('Ctrl Pts',(6.72790031412623,15.5619248294191,0.));
#10438=CARTESIAN_POINT('Ctrl Pts',(6.69953551835472,15.5083268912119,0.));
#10439=CARTESIAN_POINT('Ctrl Pts',(6.68074830397725,15.4733031879166,0.));
#10440=CARTESIAN_POINT('Ctrl Pts',(6.66297054550541,15.4424051151807,0.));
#10441=CARTESIAN_POINT('Ctrl Pts',(6.63306845520275,15.3933171197393,0.));
#10442=CARTESIAN_POINT('Ctrl Pts',(6.58832104206022,15.3282076647862,0.));
#10443=CARTESIAN_POINT('Ctrl Pts',(6.52246995302225,15.2506809503975,0.));
#10444=CARTESIAN_POINT('Ctrl Pts',(6.44397890908495,15.1795880240196,0.));
#10445=CARTESIAN_POINT('Ctrl Pts',(6.34385243988822,15.1168047097501,0.));
#10446=CARTESIAN_POINT('Ctrl Pts',(6.19604134326089,15.0680440207731,0.));
#10447=CARTESIAN_POINT('Ctrl Pts',(6.07637133495393,15.0769402326058,0.));
#10448=CARTESIAN_POINT('Ctrl Pts',(6.00933848448158,15.0980247376579,0.));
#10449=CARTESIAN_POINT('',(9.06833546026116,16.6962658094608,0.));
#10450=CARTESIAN_POINT('Origin',(0.,-2.16840434497101E-15,0.));
#10451=CARTESIAN_POINT('',(8.68235805704686,13.7360532384391,0.));
#10452=CARTESIAN_POINT('Ctrl Pts',(8.68235805704686,13.7360532384391,0.));
#10453=CARTESIAN_POINT('Ctrl Pts',(8.62589941321482,13.7778907925313,0.));
#10454=CARTESIAN_POINT('Ctrl Pts',(8.54836196063209,13.8694768008521,0.));
#10455=CARTESIAN_POINT('Ctrl Pts',(8.50092900394922,14.0177193038531,0.));
#10456=CARTESIAN_POINT('Ctrl Pts',(8.49286891019844,14.1356264252377,0.));
#10457=CARTESIAN_POINT('Ctrl Pts',(8.50424841775457,14.2409143873564,0.));
#10458=CARTESIAN_POINT('Ctrl Pts',(8.52826254822916,14.3397580968626,0.));
#10459=CARTESIAN_POINT('Ctrl Pts',(8.55463533425733,14.4142298919554,0.));
#10460=CARTESIAN_POINT('Ctrl Pts',(8.57677234909656,14.4672743909627,0.));
#10461=CARTESIAN_POINT('Ctrl Pts',(8.59131991078476,14.4998183311667,0.));
#10462=CARTESIAN_POINT('Ctrl Pts',(8.6086118344139,14.5356039231527,0.));
#10463=CARTESIAN_POINT('Ctrl Pts',(8.63530106864819,14.5900556026053,0.));
#10464=CARTESIAN_POINT('Ctrl Pts',(8.67143265073928,14.6709614647944,0.));
#10465=CARTESIAN_POINT('Ctrl Pts',(8.71655678814373,14.7823474421093,0.));
#10466=CARTESIAN_POINT('Ctrl Pts',(8.76490206435509,14.9159049694657,0.));
#10467=CARTESIAN_POINT('Ctrl Pts',(8.81495027721557,15.0719627020186,0.));
#10468=CARTESIAN_POINT('Ctrl Pts',(8.86505268915084,15.2508174554788,0.));
#10469=CARTESIAN_POINT('Ctrl Pts',(8.91357927057117,15.4526569741556,0.));
#10470=CARTESIAN_POINT('Ctrl Pts',(8.95887481023115,15.6775844882862,0.));
#10471=CARTESIAN_POINT('Ctrl Pts',(8.99927973772153,15.9256093626227,0.));
#10472=CARTESIAN_POINT('Ctrl Pts',(9.04193491022831,16.2671851013731,0.));
#10473=CARTESIAN_POINT('Ctrl Pts',(9.06094720995305,16.5270428237395,0.));
#10474=CARTESIAN_POINT('Ctrl Pts',(9.06833546026116,16.6962658094608,0.));
#10475=CARTESIAN_POINT('',(10.3807667497191,12.5020870932787,0.));
#10476=CARTESIAN_POINT('Origin',(0.,0.,0.));
#10477=CARTESIAN_POINT('',(13.07682262797,13.7839294091566,0.));
#10478=CARTESIAN_POINT('Ctrl Pts',(13.07682262797,13.7839294091566,0.));
#10479=CARTESIAN_POINT('Ctrl Pts',(12.9181650995967,13.7246099871302,0.));
#10480=CARTESIAN_POINT('Ctrl Pts',(12.6769008431476,13.6262277632565,0.));
#10481=CARTESIAN_POINT('Ctrl Pts',(12.3652241842033,13.4801075753502,0.));
#10482=CARTESIAN_POINT('Ctrl Pts',(12.1418243205134,13.3650363045723,0.));
#10483=CARTESIAN_POINT('Ctrl Pts',(11.9419026340297,13.2524512620508,0.));
#10484=CARTESIAN_POINT('Ctrl Pts',(11.764937382884,13.1439278991698,0.));
#10485=CARTESIAN_POINT('Ctrl Pts',(11.6103189008825,13.0410085154728,0.));
#10486=CARTESIAN_POINT('Ctrl Pts',(11.4773649257318,12.9451853450404,0.));
#10487=CARTESIAN_POINT('Ctrl Pts',(11.3652836809863,12.8579347093876,0.));
#10488=CARTESIAN_POINT('Ctrl Pts',(11.2732934467515,12.7805989445416,0.));
#10489=CARTESIAN_POINT('Ctrl Pts',(11.2075126722099,12.7212344815888,0.));
#10490=CARTESIAN_POINT('Ctrl Pts',(11.1639734745885,12.6790250171322,0.));
#10491=CARTESIAN_POINT('Ctrl Pts',(11.1352828524076,12.6515210644081,0.));
#10492=CARTESIAN_POINT('Ctrl Pts',(11.108827169799,12.6276288804813,0.));
#10493=CARTESIAN_POINT('Ctrl Pts',(11.0652195671547,12.5901836766158,0.));
#10494=CARTESIAN_POINT('Ctrl Pts',(11.0025423202231,12.5420886163255,0.));
#10495=CARTESIAN_POINT('Ctrl Pts',(10.9159571406242,12.48870543503,0.));
#10496=CARTESIAN_POINT('Ctrl Pts',(10.8193387993863,12.4453471106187,0.));
#10497=CARTESIAN_POINT('Ctrl Pts',(10.7047117573306,12.4165774110367,0.));
#10498=CARTESIAN_POINT('Ctrl Pts',(10.5490671691512,12.4158793808611,0.));
#10499=CARTESIAN_POINT('Ctrl Pts',(10.4380033085876,12.4613202473787,0.));
#10500=CARTESIAN_POINT('Ctrl Pts',(10.3807667497191,12.5020870932787,0.));
#10501=CARTESIAN_POINT('',(13.7839294091566,13.07682262797,0.));
#10502=CARTESIAN_POINT('Origin',(0.,0.,0.));
#10503=CARTESIAN_POINT('',(12.5020870932787,10.3807667497191,0.));
#10504=CARTESIAN_POINT('Ctrl Pts',(12.5020870932787,10.3807667497191,0.));
#10505=CARTESIAN_POINT('Ctrl Pts',(12.4613202473788,10.4380033085876,0.));
#10506=CARTESIAN_POINT('Ctrl Pts',(12.4158793808611,10.5490671691512,0.));
#10507=CARTESIAN_POINT('Ctrl Pts',(12.4165774110367,10.7047117573306,0.));
#10508=CARTESIAN_POINT('Ctrl Pts',(12.4453471106188,10.8193387993863,0.));
#10509=CARTESIAN_POINT('Ctrl Pts',(12.48870543503,10.9159571406243,0.));
#10510=CARTESIAN_POINT('Ctrl Pts',(12.5420886163255,11.0025423202231,0.));
#10511=CARTESIAN_POINT('Ctrl Pts',(12.5901836766158,11.0652195671547,0.));
#10512=CARTESIAN_POINT('Ctrl Pts',(12.6276288804813,11.1088271697991,0.));
#10513=CARTESIAN_POINT('Ctrl Pts',(12.651521064408,11.1352828524077,0.));
#10514=CARTESIAN_POINT('Ctrl Pts',(12.6790250171322,11.1639734745885,0.));
#10515=CARTESIAN_POINT('Ctrl Pts',(12.7212344815888,11.2075126722099,0.));
#10516=CARTESIAN_POINT('Ctrl Pts',(12.7805989445416,11.2732934467515,0.));
#10517=CARTESIAN_POINT('Ctrl Pts',(12.8579347093876,11.3652836809863,0.));
#10518=CARTESIAN_POINT('Ctrl Pts',(12.9451853450404,11.4773649257318,0.));
#10519=CARTESIAN_POINT('Ctrl Pts',(13.0410085154727,11.6103189008825,0.));
#10520=CARTESIAN_POINT('Ctrl Pts',(13.1439278991698,11.764937382884,0.));
#10521=CARTESIAN_POINT('Ctrl Pts',(13.2524512620507,11.9419026340297,0.));
#10522=CARTESIAN_POINT('Ctrl Pts',(13.3650363045724,12.1418243205134,0.));
#10523=CARTESIAN_POINT('Ctrl Pts',(13.4801075753502,12.3652241842034,0.));
#10524=CARTESIAN_POINT('Ctrl Pts',(13.6262277632565,12.6769008431476,0.));
#10525=CARTESIAN_POINT('Ctrl Pts',(13.7246099871303,12.9181650995967,0.));
#10526=CARTESIAN_POINT('Ctrl Pts',(13.7839294091566,13.07682262797,0.));
#10527=CARTESIAN_POINT('',(13.7360532384392,8.6823580570467,0.));
#10528=CARTESIAN_POINT('Origin',(0.,0.,0.));
#10529=CARTESIAN_POINT('',(16.6962658094608,9.06833546026115,0.));
#10530=CARTESIAN_POINT('Ctrl Pts',(16.6962658094608,9.06833546026115,0.));
#10531=CARTESIAN_POINT('Ctrl Pts',(16.5270428237395,9.06094720995301,0.));
#10532=CARTESIAN_POINT('Ctrl Pts',(16.267185101373,9.0419349102283,0.));
#10533=CARTESIAN_POINT('Ctrl Pts',(15.9256093626227,8.9992797377215,0.));
#10534=CARTESIAN_POINT('Ctrl Pts',(15.6775844882862,8.95887481023115,0.));
#10535=CARTESIAN_POINT('Ctrl Pts',(15.4526569741556,8.9135792705712,0.));
#10536=CARTESIAN_POINT('Ctrl Pts',(15.2508174554787,8.86505268915081,0.));
#10537=CARTESIAN_POINT('Ctrl Pts',(15.0719627020186,8.8149502772156,0.));
#10538=CARTESIAN_POINT('Ctrl Pts',(14.9159049694657,8.76490206435509,0.));
#10539=CARTESIAN_POINT('Ctrl Pts',(14.7823474421092,8.71655678814372,0.));
#10540=CARTESIAN_POINT('Ctrl Pts',(14.6709614647943,8.67143265073928,0.));
#10541=CARTESIAN_POINT('Ctrl Pts',(14.5900556026053,8.63530106864818,0.));
#10542=CARTESIAN_POINT('Ctrl Pts',(14.5356039231526,8.60861183441388,0.));
#10543=CARTESIAN_POINT('Ctrl Pts',(14.4998183311667,8.59131991078479,0.));
#10544=CARTESIAN_POINT('Ctrl Pts',(14.4672743909626,8.57677234909658,0.));
#10545=CARTESIAN_POINT('Ctrl Pts',(14.4142298919554,8.55463533425733,0.));
#10546=CARTESIAN_POINT('Ctrl Pts',(14.3397580968625,8.52826254822916,0.));
#10547=CARTESIAN_POINT('Ctrl Pts',(14.2409143873564,8.50424841775457,0.));
#10548=CARTESIAN_POINT('Ctrl Pts',(14.1356264252376,8.49286891019843,0.));
#10549=CARTESIAN_POINT('Ctrl Pts',(14.0177193038531,8.5009290039492,0.));
#10550=CARTESIAN_POINT('Ctrl Pts',(13.8694768008521,8.54836196063209,0.));
#10551=CARTESIAN_POINT('Ctrl Pts',(13.7778907925312,8.62589941321481,0.));
#10552=CARTESIAN_POINT('Ctrl Pts',(13.7360532384392,8.6823580570467,0.));
#10553=CARTESIAN_POINT('Origin',(2.16840434497101E-15,0.,0.));
#10554=CARTESIAN_POINT('Ctrl Pts',(15.0980247376579,6.00933848448159,7.));
#10555=CARTESIAN_POINT('Ctrl Pts',(15.0980247376579,6.00933848448159,-1.4));
#10556=CARTESIAN_POINT('Ctrl Pts',(15.0769402326058,6.07637133495396,7.));
#10557=CARTESIAN_POINT('Ctrl Pts',(15.0769402326058,6.07637133495396,-1.4));
#10558=CARTESIAN_POINT('Ctrl Pts',(15.0680440207731,6.1960413432609,7.));
#10559=CARTESIAN_POINT('Ctrl Pts',(15.0680440207731,6.1960413432609,-1.4));
#10560=CARTESIAN_POINT('Ctrl Pts',(15.1168047097502,6.34385243988821,7.));
#10561=CARTESIAN_POINT('Ctrl Pts',(15.1168047097502,6.34385243988821,-1.4));
#10562=CARTESIAN_POINT('Ctrl Pts',(15.1795880240196,6.44397890908497,7.));
#10563=CARTESIAN_POINT('Ctrl Pts',(15.1795880240196,6.44397890908497,-1.4));
#10564=CARTESIAN_POINT('Ctrl Pts',(15.2506809503975,6.52246995302229,7.));
#10565=CARTESIAN_POINT('Ctrl Pts',(15.2506809503975,6.52246995302229,-1.4));
#10566=CARTESIAN_POINT('Ctrl Pts',(15.3282076647862,6.58832104206024,7.));
#10567=CARTESIAN_POINT('Ctrl Pts',(15.3282076647862,6.58832104206024,-1.4));
#10568=CARTESIAN_POINT('Ctrl Pts',(15.3933171197393,6.63306845520277,7.));
#10569=CARTESIAN_POINT('Ctrl Pts',(15.3933171197393,6.63306845520277,-1.4));
#10570=CARTESIAN_POINT('Ctrl Pts',(15.4424051151807,6.66297054550544,7.));
#10571=CARTESIAN_POINT('Ctrl Pts',(15.4424051151807,6.66297054550544,-1.4));
#10572=CARTESIAN_POINT('Ctrl Pts',(15.4733031879166,6.68074830397728,7.));
#10573=CARTESIAN_POINT('Ctrl Pts',(15.4733031879166,6.68074830397728,-1.4));
#10574=CARTESIAN_POINT('Ctrl Pts',(15.5083268912119,6.69953551835471,7.));
#10575=CARTESIAN_POINT('Ctrl Pts',(15.5083268912119,6.69953551835471,-1.4));
#10576=CARTESIAN_POINT('Ctrl Pts',(15.5619248294191,6.72790031412625,7.));
#10577=CARTESIAN_POINT('Ctrl Pts',(15.5619248294191,6.72790031412625,-1.4));
#10578=CARTESIAN_POINT('Ctrl Pts',(15.6387111659832,6.77211692048664,7.));
#10579=CARTESIAN_POINT('Ctrl Pts',(15.6387111659832,6.77211692048664,-1.4));
#10580=CARTESIAN_POINT('Ctrl Pts',(15.7406883947778,6.83570676658069,7.));
#10581=CARTESIAN_POINT('Ctrl Pts',(15.7406883947778,6.83570676658069,-1.4));
#10582=CARTESIAN_POINT('Ctrl Pts',(15.8583036897433,6.91534043556371,7.));
#10583=CARTESIAN_POINT('Ctrl Pts',(15.8583036897433,6.91534043556371,-1.4));
#10584=CARTESIAN_POINT('Ctrl Pts',(15.9905219781863,7.01217619187965,7.));
#10585=CARTESIAN_POINT('Ctrl Pts',(15.9905219781863,7.01217619187965,-1.4));
#10586=CARTESIAN_POINT('Ctrl Pts',(16.1361838672874,7.12742326811382,7.));
#10587=CARTESIAN_POINT('Ctrl Pts',(16.1361838672874,7.12742326811382,-1.4));
#10588=CARTESIAN_POINT('Ctrl Pts',(16.2940809887434,7.2621916599568,7.));
#10589=CARTESIAN_POINT('Ctrl Pts',(16.2940809887434,7.2621916599568,-1.4));
#10590=CARTESIAN_POINT('Ctrl Pts',(16.4629349257385,7.41753779118422,7.));
#10591=CARTESIAN_POINT('Ctrl Pts',(16.4629349257385,7.41753779118422,-1.4));
#10592=CARTESIAN_POINT('Ctrl Pts',(16.6414085620714,7.59444470905136,7.));
#10593=CARTESIAN_POINT('Ctrl Pts',(16.6414085620714,7.59444470905136,-1.4));
#10594=CARTESIAN_POINT('Ctrl Pts',(16.8766905033057,7.84571320523309,7.));
#10595=CARTESIAN_POINT('Ctrl Pts',(16.8766905033057,7.84571320523309,-1.4));
#10596=CARTESIAN_POINT('Ctrl Pts',(17.0448123137865,8.04476736935674,7.));
#10597=CARTESIAN_POINT('Ctrl Pts',(17.0448123137865,8.04476736935674,-1.4));
#10598=CARTESIAN_POINT('Ctrl Pts',(17.1502563092004,8.1773289360728,7.));
#10599=CARTESIAN_POINT('Ctrl Pts',(17.1502563092004,8.1773289360728,-1.4));
#10600=CARTESIAN_POINT('',(17.1502563092004,8.17732893607278,7.));
#10601=CARTESIAN_POINT('',(15.0980247376579,6.00933848448158,7.));
#10602=CARTESIAN_POINT('Origin',(2.16840434497101E-15,0.,7.));
#10603=CARTESIAN_POINT('',(16.6962658094608,9.06833546026115,7.));
#10604=CARTESIAN_POINT('Ctrl Pts',(16.6962658094608,9.06833546026116,7.));
#10605=CARTESIAN_POINT('Ctrl Pts',(16.6962658094608,9.06833546026116,-1.39999999999999));
#10606=CARTESIAN_POINT('Ctrl Pts',(16.5270428237395,9.06094720995301,7.));
#10607=CARTESIAN_POINT('Ctrl Pts',(16.5270428237395,9.06094720995301,-1.39999999999999));
#10608=CARTESIAN_POINT('Ctrl Pts',(16.267185101373,9.0419349102283,7.));
#10609=CARTESIAN_POINT('Ctrl Pts',(16.267185101373,9.0419349102283,-1.39999999999999));
#10610=CARTESIAN_POINT('Ctrl Pts',(15.9256093626227,8.9992797377215,7.));
#10611=CARTESIAN_POINT('Ctrl Pts',(15.9256093626227,8.9992797377215,-1.39999999999999));
#10612=CARTESIAN_POINT('Ctrl Pts',(15.6775844882862,8.95887481023115,7.));
#10613=CARTESIAN_POINT('Ctrl Pts',(15.6775844882862,8.95887481023115,-1.39999999999999));
#10614=CARTESIAN_POINT('Ctrl Pts',(15.4526569741556,8.9135792705712,7.));
#10615=CARTESIAN_POINT('Ctrl Pts',(15.4526569741556,8.9135792705712,-1.39999999999999));
#10616=CARTESIAN_POINT('Ctrl Pts',(15.2508174554787,8.86505268915081,7.));
#10617=CARTESIAN_POINT('Ctrl Pts',(15.2508174554787,8.86505268915081,-1.39999999999999));
#10618=CARTESIAN_POINT('Ctrl Pts',(15.0719627020186,8.8149502772156,7.));
#10619=CARTESIAN_POINT('Ctrl Pts',(15.0719627020186,8.8149502772156,-1.39999999999999));
#10620=CARTESIAN_POINT('Ctrl Pts',(14.9159049694657,8.76490206435509,7.));
#10621=CARTESIAN_POINT('Ctrl Pts',(14.9159049694657,8.76490206435509,-1.39999999999999));
#10622=CARTESIAN_POINT('Ctrl Pts',(14.7823474421092,8.71655678814372,7.));
#10623=CARTESIAN_POINT('Ctrl Pts',(14.7823474421092,8.71655678814372,-1.39999999999999));
#10624=CARTESIAN_POINT('Ctrl Pts',(14.6709614647943,8.67143265073928,7.));
#10625=CARTESIAN_POINT('Ctrl Pts',(14.6709614647943,8.67143265073928,-1.39999999999999));
#10626=CARTESIAN_POINT('Ctrl Pts',(14.5900556026053,8.63530106864818,7.));
#10627=CARTESIAN_POINT('Ctrl Pts',(14.5900556026053,8.63530106864818,-1.39999999999999));
#10628=CARTESIAN_POINT('Ctrl Pts',(14.5356039231526,8.60861183441388,7.));
#10629=CARTESIAN_POINT('Ctrl Pts',(14.5356039231526,8.60861183441388,-1.39999999999999));
#10630=CARTESIAN_POINT('Ctrl Pts',(14.4998183311667,8.59131991078479,7.));
#10631=CARTESIAN_POINT('Ctrl Pts',(14.4998183311667,8.59131991078479,-1.39999999999999));
#10632=CARTESIAN_POINT('Ctrl Pts',(14.4672743909626,8.57677234909658,7.));
#10633=CARTESIAN_POINT('Ctrl Pts',(14.4672743909626,8.57677234909658,-1.39999999999999));
#10634=CARTESIAN_POINT('Ctrl Pts',(14.4142298919554,8.55463533425733,7.));
#10635=CARTESIAN_POINT('Ctrl Pts',(14.4142298919554,8.55463533425733,-1.39999999999999));
#10636=CARTESIAN_POINT('Ctrl Pts',(14.3397580968625,8.52826254822916,7.));
#10637=CARTESIAN_POINT('Ctrl Pts',(14.3397580968625,8.52826254822916,-1.39999999999999));
#10638=CARTESIAN_POINT('Ctrl Pts',(14.2409143873564,8.50424841775457,7.));
#10639=CARTESIAN_POINT('Ctrl Pts',(14.2409143873564,8.50424841775457,-1.39999999999999));
#10640=CARTESIAN_POINT('Ctrl Pts',(14.1356264252376,8.49286891019843,7.));
#10641=CARTESIAN_POINT('Ctrl Pts',(14.1356264252376,8.49286891019843,-1.39999999999999));
#10642=CARTESIAN_POINT('Ctrl Pts',(14.0177193038531,8.5009290039492,7.));
#10643=CARTESIAN_POINT('Ctrl Pts',(14.0177193038531,8.5009290039492,-1.39999999999999));
#10644=CARTESIAN_POINT('Ctrl Pts',(13.8694768008521,8.54836196063209,7.));
#10645=CARTESIAN_POINT('Ctrl Pts',(13.8694768008521,8.54836196063209,-1.39999999999999));
#10646=CARTESIAN_POINT('Ctrl Pts',(13.7778907925312,8.62589941321481,7.));
#10647=CARTESIAN_POINT('Ctrl Pts',(13.7778907925312,8.62589941321481,-1.39999999999999));
#10648=CARTESIAN_POINT('Ctrl Pts',(13.7360532384392,8.6823580570467,7.));
#10649=CARTESIAN_POINT('Ctrl Pts',(13.7360532384392,8.6823580570467,-1.39999999999999));
#10650=CARTESIAN_POINT('',(13.7360532384392,8.6823580570467,7.));
#10651=CARTESIAN_POINT('Origin',(0.,0.,7.));
#10652=CARTESIAN_POINT('',(12.5020870932787,10.3807667497191,7.));
#10653=CARTESIAN_POINT('Ctrl Pts',(12.5020870932787,10.3807667497191,7.));
#10654=CARTESIAN_POINT('Ctrl Pts',(12.5020870932787,10.3807667497191,-1.4));
#10655=CARTESIAN_POINT('Ctrl Pts',(12.4613202473788,10.4380033085876,7.));
#10656=CARTESIAN_POINT('Ctrl Pts',(12.4613202473788,10.4380033085876,-1.4));
#10657=CARTESIAN_POINT('Ctrl Pts',(12.4158793808611,10.5490671691512,7.));
#10658=CARTESIAN_POINT('Ctrl Pts',(12.4158793808611,10.5490671691512,-1.4));
#10659=CARTESIAN_POINT('Ctrl Pts',(12.4165774110367,10.7047117573306,7.));
#10660=CARTESIAN_POINT('Ctrl Pts',(12.4165774110367,10.7047117573306,-1.4));
#10661=CARTESIAN_POINT('Ctrl Pts',(12.4453471106188,10.8193387993863,7.));
#10662=CARTESIAN_POINT('Ctrl Pts',(12.4453471106188,10.8193387993863,-1.4));
#10663=CARTESIAN_POINT('Ctrl Pts',(12.48870543503,10.9159571406243,7.));
#10664=CARTESIAN_POINT('Ctrl Pts',(12.48870543503,10.9159571406243,-1.4));
#10665=CARTESIAN_POINT('Ctrl Pts',(12.5420886163255,11.0025423202231,7.));
#10666=CARTESIAN_POINT('Ctrl Pts',(12.5420886163255,11.0025423202231,-1.4));
#10667=CARTESIAN_POINT('Ctrl Pts',(12.5901836766158,11.0652195671547,7.));
#10668=CARTESIAN_POINT('Ctrl Pts',(12.5901836766158,11.0652195671547,-1.4));
#10669=CARTESIAN_POINT('Ctrl Pts',(12.6276288804813,11.1088271697991,7.));
#10670=CARTESIAN_POINT('Ctrl Pts',(12.6276288804813,11.1088271697991,-1.4));
#10671=CARTESIAN_POINT('Ctrl Pts',(12.651521064408,11.1352828524077,7.));
#10672=CARTESIAN_POINT('Ctrl Pts',(12.651521064408,11.1352828524077,-1.4));
#10673=CARTESIAN_POINT('Ctrl Pts',(12.6790250171322,11.1639734745885,7.));
#10674=CARTESIAN_POINT('Ctrl Pts',(12.6790250171322,11.1639734745885,-1.4));
#10675=CARTESIAN_POINT('Ctrl Pts',(12.7212344815888,11.2075126722099,7.));
#10676=CARTESIAN_POINT('Ctrl Pts',(12.7212344815888,11.2075126722099,-1.4));
#10677=CARTESIAN_POINT('Ctrl Pts',(12.7805989445416,11.2732934467515,7.));
#10678=CARTESIAN_POINT('Ctrl Pts',(12.7805989445416,11.2732934467515,-1.4));
#10679=CARTESIAN_POINT('Ctrl Pts',(12.8579347093876,11.3652836809863,7.));
#10680=CARTESIAN_POINT('Ctrl Pts',(12.8579347093876,11.3652836809863,-1.4));
#10681=CARTESIAN_POINT('Ctrl Pts',(12.9451853450404,11.4773649257318,7.));
#10682=CARTESIAN_POINT('Ctrl Pts',(12.9451853450404,11.4773649257318,-1.4));
#10683=CARTESIAN_POINT('Ctrl Pts',(13.0410085154727,11.6103189008825,7.));
#10684=CARTESIAN_POINT('Ctrl Pts',(13.0410085154727,11.6103189008825,-1.4));
#10685=CARTESIAN_POINT('Ctrl Pts',(13.1439278991698,11.764937382884,7.));
#10686=CARTESIAN_POINT('Ctrl Pts',(13.1439278991698,11.764937382884,-1.4));
#10687=CARTESIAN_POINT('Ctrl Pts',(13.2524512620507,11.9419026340297,7.));
#10688=CARTESIAN_POINT('Ctrl Pts',(13.2524512620507,11.9419026340297,-1.4));
#10689=CARTESIAN_POINT('Ctrl Pts',(13.3650363045724,12.1418243205134,7.));
#10690=CARTESIAN_POINT('Ctrl Pts',(13.3650363045724,12.1418243205134,-1.4));
#10691=CARTESIAN_POINT('Ctrl Pts',(13.4801075753502,12.3652241842034,7.));
#10692=CARTESIAN_POINT('Ctrl Pts',(13.4801075753502,12.3652241842034,-1.4));
#10693=CARTESIAN_POINT('Ctrl Pts',(13.6262277632565,12.6769008431476,7.));
#10694=CARTESIAN_POINT('Ctrl Pts',(13.6262277632565,12.6769008431476,-1.4));
#10695=CARTESIAN_POINT('Ctrl Pts',(13.7246099871303,12.9181650995967,7.));
#10696=CARTESIAN_POINT('Ctrl Pts',(13.7246099871303,12.9181650995967,-1.4));
#10697=CARTESIAN_POINT('Ctrl Pts',(13.7839294091566,13.07682262797,7.));
#10698=CARTESIAN_POINT('Ctrl Pts',(13.7839294091566,13.07682262797,-1.4));
#10699=CARTESIAN_POINT('',(13.7839294091566,13.07682262797,7.));
#10700=CARTESIAN_POINT('Origin',(0.,0.,7.));
#10701=CARTESIAN_POINT('',(13.07682262797,13.7839294091566,7.));
#10702=CARTESIAN_POINT('Ctrl Pts',(13.07682262797,13.7839294091566,7.));
#10703=CARTESIAN_POINT('Ctrl Pts',(13.07682262797,13.7839294091566,-1.39999999999998));
#10704=CARTESIAN_POINT('Ctrl Pts',(12.9181650995967,13.7246099871302,7.));
#10705=CARTESIAN_POINT('Ctrl Pts',(12.9181650995967,13.7246099871302,-1.39999999999998));
#10706=CARTESIAN_POINT('Ctrl Pts',(12.6769008431476,13.6262277632565,7.));
#10707=CARTESIAN_POINT('Ctrl Pts',(12.6769008431476,13.6262277632565,-1.39999999999998));
#10708=CARTESIAN_POINT('Ctrl Pts',(12.3652241842033,13.4801075753502,7.));
#10709=CARTESIAN_POINT('Ctrl Pts',(12.3652241842033,13.4801075753502,-1.39999999999998));
#10710=CARTESIAN_POINT('Ctrl Pts',(12.1418243205134,13.3650363045723,7.));
#10711=CARTESIAN_POINT('Ctrl Pts',(12.1418243205134,13.3650363045723,-1.39999999999998));
#10712=CARTESIAN_POINT('Ctrl Pts',(11.9419026340297,13.2524512620508,7.));
#10713=CARTESIAN_POINT('Ctrl Pts',(11.9419026340297,13.2524512620508,-1.39999999999998));
#10714=CARTESIAN_POINT('Ctrl Pts',(11.764937382884,13.1439278991698,7.));
#10715=CARTESIAN_POINT('Ctrl Pts',(11.764937382884,13.1439278991698,-1.39999999999998));
#10716=CARTESIAN_POINT('Ctrl Pts',(11.6103189008825,13.0410085154728,7.));
#10717=CARTESIAN_POINT('Ctrl Pts',(11.6103189008825,13.0410085154728,-1.39999999999998));
#10718=CARTESIAN_POINT('Ctrl Pts',(11.4773649257318,12.9451853450404,7.));
#10719=CARTESIAN_POINT('Ctrl Pts',(11.4773649257318,12.9451853450404,-1.39999999999998));
#10720=CARTESIAN_POINT('Ctrl Pts',(11.3652836809863,12.8579347093876,7.));
#10721=CARTESIAN_POINT('Ctrl Pts',(11.3652836809863,12.8579347093876,-1.39999999999998));
#10722=CARTESIAN_POINT('Ctrl Pts',(11.2732934467515,12.7805989445416,7.));
#10723=CARTESIAN_POINT('Ctrl Pts',(11.2732934467515,12.7805989445416,-1.39999999999998));
#10724=CARTESIAN_POINT('Ctrl Pts',(11.2075126722099,12.7212344815888,7.));
#10725=CARTESIAN_POINT('Ctrl Pts',(11.2075126722099,12.7212344815888,-1.39999999999998));
#10726=CARTESIAN_POINT('Ctrl Pts',(11.1639734745885,12.6790250171322,7.));
#10727=CARTESIAN_POINT('Ctrl Pts',(11.1639734745885,12.6790250171322,-1.39999999999998));
#10728=CARTESIAN_POINT('Ctrl Pts',(11.1352828524076,12.6515210644081,7.));
#10729=CARTESIAN_POINT('Ctrl Pts',(11.1352828524076,12.6515210644081,-1.39999999999998));
#10730=CARTESIAN_POINT('Ctrl Pts',(11.108827169799,12.6276288804813,7.));
#10731=CARTESIAN_POINT('Ctrl Pts',(11.108827169799,12.6276288804813,-1.39999999999998));
#10732=CARTESIAN_POINT('Ctrl Pts',(11.0652195671547,12.5901836766158,7.));
#10733=CARTESIAN_POINT('Ctrl Pts',(11.0652195671547,12.5901836766158,-1.39999999999998));
#10734=CARTESIAN_POINT('Ctrl Pts',(11.0025423202231,12.5420886163255,7.));
#10735=CARTESIAN_POINT('Ctrl Pts',(11.0025423202231,12.5420886163255,-1.39999999999998));
#10736=CARTESIAN_POINT('Ctrl Pts',(10.9159571406242,12.48870543503,7.));
#10737=CARTESIAN_POINT('Ctrl Pts',(10.9159571406242,12.48870543503,-1.39999999999998));
#10738=CARTESIAN_POINT('Ctrl Pts',(10.8193387993863,12.4453471106187,7.));
#10739=CARTESIAN_POINT('Ctrl Pts',(10.8193387993863,12.4453471106187,-1.39999999999998));
#10740=CARTESIAN_POINT('Ctrl Pts',(10.7047117573306,12.4165774110367,7.));
#10741=CARTESIAN_POINT('Ctrl Pts',(10.7047117573306,12.4165774110367,-1.39999999999998));
#10742=CARTESIAN_POINT('Ctrl Pts',(10.5490671691512,12.4158793808611,7.));
#10743=CARTESIAN_POINT('Ctrl Pts',(10.5490671691512,12.4158793808611,-1.39999999999998));
#10744=CARTESIAN_POINT('Ctrl Pts',(10.4380033085876,12.4613202473787,7.));
#10745=CARTESIAN_POINT('Ctrl Pts',(10.4380033085876,12.4613202473787,-1.39999999999998));
#10746=CARTESIAN_POINT('Ctrl Pts',(10.3807667497191,12.5020870932787,7.));
#10747=CARTESIAN_POINT('Ctrl Pts',(10.3807667497191,12.5020870932787,-1.39999999999998));
#10748=CARTESIAN_POINT('',(10.3807667497191,12.5020870932787,7.));
#10749=CARTESIAN_POINT('Origin',(0.,0.,7.));
#10750=CARTESIAN_POINT('',(8.68235805704686,13.7360532384391,7.));
#10751=CARTESIAN_POINT('Ctrl Pts',(8.68235805704669,13.7360532384392,7.));
#10752=CARTESIAN_POINT('Ctrl Pts',(8.68235805704669,13.7360532384392,-1.4));
#10753=CARTESIAN_POINT('Ctrl Pts',(8.62589941321482,13.7778907925313,7.));
#10754=CARTESIAN_POINT('Ctrl Pts',(8.62589941321482,13.7778907925313,-1.4));
#10755=CARTESIAN_POINT('Ctrl Pts',(8.54836196063209,13.8694768008521,7.));
#10756=CARTESIAN_POINT('Ctrl Pts',(8.54836196063209,13.8694768008521,-1.4));
#10757=CARTESIAN_POINT('Ctrl Pts',(8.50092900394922,14.0177193038531,7.));
#10758=CARTESIAN_POINT('Ctrl Pts',(8.50092900394922,14.0177193038531,-1.4));
#10759=CARTESIAN_POINT('Ctrl Pts',(8.49286891019844,14.1356264252377,7.));
#10760=CARTESIAN_POINT('Ctrl Pts',(8.49286891019844,14.1356264252377,-1.4));
#10761=CARTESIAN_POINT('Ctrl Pts',(8.50424841775457,14.2409143873564,7.));
#10762=CARTESIAN_POINT('Ctrl Pts',(8.50424841775457,14.2409143873564,-1.4));
#10763=CARTESIAN_POINT('Ctrl Pts',(8.52826254822916,14.3397580968626,7.));
#10764=CARTESIAN_POINT('Ctrl Pts',(8.52826254822916,14.3397580968626,-1.4));
#10765=CARTESIAN_POINT('Ctrl Pts',(8.55463533425733,14.4142298919554,7.));
#10766=CARTESIAN_POINT('Ctrl Pts',(8.55463533425733,14.4142298919554,-1.4));
#10767=CARTESIAN_POINT('Ctrl Pts',(8.57677234909656,14.4672743909627,7.));
#10768=CARTESIAN_POINT('Ctrl Pts',(8.57677234909656,14.4672743909627,-1.4));
#10769=CARTESIAN_POINT('Ctrl Pts',(8.59131991078476,14.4998183311667,7.));
#10770=CARTESIAN_POINT('Ctrl Pts',(8.59131991078476,14.4998183311667,-1.4));
#10771=CARTESIAN_POINT('Ctrl Pts',(8.6086118344139,14.5356039231527,7.));
#10772=CARTESIAN_POINT('Ctrl Pts',(8.6086118344139,14.5356039231527,-1.4));
#10773=CARTESIAN_POINT('Ctrl Pts',(8.63530106864819,14.5900556026053,7.));
#10774=CARTESIAN_POINT('Ctrl Pts',(8.63530106864819,14.5900556026053,-1.4));
#10775=CARTESIAN_POINT('Ctrl Pts',(8.67143265073928,14.6709614647944,7.));
#10776=CARTESIAN_POINT('Ctrl Pts',(8.67143265073928,14.6709614647944,-1.4));
#10777=CARTESIAN_POINT('Ctrl Pts',(8.71655678814373,14.7823474421093,7.));
#10778=CARTESIAN_POINT('Ctrl Pts',(8.71655678814373,14.7823474421093,-1.4));
#10779=CARTESIAN_POINT('Ctrl Pts',(8.76490206435509,14.9159049694657,7.));
#10780=CARTESIAN_POINT('Ctrl Pts',(8.76490206435509,14.9159049694657,-1.4));
#10781=CARTESIAN_POINT('Ctrl Pts',(8.81495027721557,15.0719627020186,7.));
#10782=CARTESIAN_POINT('Ctrl Pts',(8.81495027721557,15.0719627020186,-1.4));
#10783=CARTESIAN_POINT('Ctrl Pts',(8.86505268915084,15.2508174554788,7.));
#10784=CARTESIAN_POINT('Ctrl Pts',(8.86505268915084,15.2508174554788,-1.4));
#10785=CARTESIAN_POINT('Ctrl Pts',(8.91357927057117,15.4526569741556,7.));
#10786=CARTESIAN_POINT('Ctrl Pts',(8.91357927057117,15.4526569741556,-1.4));
#10787=CARTESIAN_POINT('Ctrl Pts',(8.95887481023115,15.6775844882862,7.));
#10788=CARTESIAN_POINT('Ctrl Pts',(8.95887481023115,15.6775844882862,-1.4));
#10789=CARTESIAN_POINT('Ctrl Pts',(8.99927973772153,15.9256093626227,7.));
#10790=CARTESIAN_POINT('Ctrl Pts',(8.99927973772153,15.9256093626227,-1.4));
#10791=CARTESIAN_POINT('Ctrl Pts',(9.04193491022831,16.2671851013731,7.));
#10792=CARTESIAN_POINT('Ctrl Pts',(9.04193491022831,16.2671851013731,-1.4));
#10793=CARTESIAN_POINT('Ctrl Pts',(9.06094720995305,16.5270428237395,7.));
#10794=CARTESIAN_POINT('Ctrl Pts',(9.06094720995305,16.5270428237395,-1.4));
#10795=CARTESIAN_POINT('Ctrl Pts',(9.06833546026116,16.6962658094608,7.));
#10796=CARTESIAN_POINT('Ctrl Pts',(9.06833546026116,16.6962658094608,-1.4));
#10797=CARTESIAN_POINT('',(9.06833546026116,16.6962658094608,7.));
#10798=CARTESIAN_POINT('Origin',(0.,-2.16840434497101E-15,7.));
#10799=CARTESIAN_POINT('',(8.17732893607301,17.1502563092002,7.));
#10800=CARTESIAN_POINT('Ctrl Pts',(8.17732893607279,17.1502563092004,7.));
#10801=CARTESIAN_POINT('Ctrl Pts',(8.17732893607279,17.1502563092004,-1.39999999999999));
#10802=CARTESIAN_POINT('Ctrl Pts',(8.04476736935673,17.0448123137865,7.));
#10803=CARTESIAN_POINT('Ctrl Pts',(8.04476736935673,17.0448123137865,-1.39999999999999));
#10804=CARTESIAN_POINT('Ctrl Pts',(7.84571320523309,16.8766905033057,7.));
#10805=CARTESIAN_POINT('Ctrl Pts',(7.84571320523309,16.8766905033057,-1.39999999999999));
#10806=CARTESIAN_POINT('Ctrl Pts',(7.59444470905135,16.6414085620714,7.));
#10807=CARTESIAN_POINT('Ctrl Pts',(7.59444470905135,16.6414085620714,-1.39999999999999));
#10808=CARTESIAN_POINT('Ctrl Pts',(7.4175377911842,16.4629349257385,7.));
#10809=CARTESIAN_POINT('Ctrl Pts',(7.4175377911842,16.4629349257385,-1.39999999999999));
#10810=CARTESIAN_POINT('Ctrl Pts',(7.26219165995678,16.2940809887434,7.));
#10811=CARTESIAN_POINT('Ctrl Pts',(7.26219165995678,16.2940809887434,-1.39999999999999));
#10812=CARTESIAN_POINT('Ctrl Pts',(7.12742326811382,16.1361838672874,7.));
#10813=CARTESIAN_POINT('Ctrl Pts',(7.12742326811382,16.1361838672874,-1.39999999999999));
#10814=CARTESIAN_POINT('Ctrl Pts',(7.01217619187961,15.9905219781863,7.));
#10815=CARTESIAN_POINT('Ctrl Pts',(7.01217619187961,15.9905219781863,-1.39999999999999));
#10816=CARTESIAN_POINT('Ctrl Pts',(6.91534043556368,15.8583036897433,7.));
#10817=CARTESIAN_POINT('Ctrl Pts',(6.91534043556368,15.8583036897433,-1.39999999999999));
#10818=CARTESIAN_POINT('Ctrl Pts',(6.83570676658068,15.7406883947777,7.));
#10819=CARTESIAN_POINT('Ctrl Pts',(6.83570676658068,15.7406883947777,-1.39999999999999));
#10820=CARTESIAN_POINT('Ctrl Pts',(6.77211692048662,15.6387111659832,7.));
#10821=CARTESIAN_POINT('Ctrl Pts',(6.77211692048662,15.6387111659832,-1.39999999999999));
#10822=CARTESIAN_POINT('Ctrl Pts',(6.72790031412623,15.5619248294191,7.));
#10823=CARTESIAN_POINT('Ctrl Pts',(6.72790031412623,15.5619248294191,-1.39999999999999));
#10824=CARTESIAN_POINT('Ctrl Pts',(6.69953551835472,15.5083268912119,7.));
#10825=CARTESIAN_POINT('Ctrl Pts',(6.69953551835472,15.5083268912119,-1.39999999999999));
#10826=CARTESIAN_POINT('Ctrl Pts',(6.68074830397725,15.4733031879166,7.));
#10827=CARTESIAN_POINT('Ctrl Pts',(6.68074830397725,15.4733031879166,-1.39999999999999));
#10828=CARTESIAN_POINT('Ctrl Pts',(6.66297054550541,15.4424051151807,7.));
#10829=CARTESIAN_POINT('Ctrl Pts',(6.66297054550541,15.4424051151807,-1.39999999999999));
#10830=CARTESIAN_POINT('Ctrl Pts',(6.63306845520275,15.3933171197393,7.));
#10831=CARTESIAN_POINT('Ctrl Pts',(6.63306845520275,15.3933171197393,-1.39999999999999));
#10832=CARTESIAN_POINT('Ctrl Pts',(6.58832104206022,15.3282076647862,7.));
#10833=CARTESIAN_POINT('Ctrl Pts',(6.58832104206022,15.3282076647862,-1.39999999999999));
#10834=CARTESIAN_POINT('Ctrl Pts',(6.52246995302225,15.2506809503975,7.));
#10835=CARTESIAN_POINT('Ctrl Pts',(6.52246995302225,15.2506809503975,-1.39999999999999));
#10836=CARTESIAN_POINT('Ctrl Pts',(6.44397890908495,15.1795880240196,7.));
#10837=CARTESIAN_POINT('Ctrl Pts',(6.44397890908495,15.1795880240196,-1.39999999999999));
#10838=CARTESIAN_POINT('Ctrl Pts',(6.34385243988822,15.1168047097501,7.));
#10839=CARTESIAN_POINT('Ctrl Pts',(6.34385243988822,15.1168047097501,-1.39999999999999));
#10840=CARTESIAN_POINT('Ctrl Pts',(6.19604134326089,15.0680440207731,7.));
#10841=CARTESIAN_POINT('Ctrl Pts',(6.19604134326089,15.0680440207731,-1.39999999999999));
#10842=CARTESIAN_POINT('Ctrl Pts',(6.07637133495393,15.0769402326058,7.));
#10843=CARTESIAN_POINT('Ctrl Pts',(6.07637133495393,15.0769402326058,-1.39999999999999));
#10844=CARTESIAN_POINT('Ctrl Pts',(6.00933848448158,15.0980247376579,7.));
#10845=CARTESIAN_POINT('Ctrl Pts',(6.00933848448158,15.0980247376579,-1.39999999999999));
#10846=CARTESIAN_POINT('',(6.00933848448158,15.0980247376579,7.));
#10847=CARTESIAN_POINT('Origin',(0.,0.,7.));
#10848=CARTESIAN_POINT('',(4.01273932064543,15.7467591314704,7.));
#10849=CARTESIAN_POINT('Ctrl Pts',(4.01273932064519,15.7467591314705,7.));
#10850=CARTESIAN_POINT('Ctrl Pts',(4.01273932064519,15.7467591314705,-1.40000000000002));
#10851=CARTESIAN_POINT('Ctrl Pts',(3.94611544431017,15.7691023294921,7.));
#10852=CARTESIAN_POINT('Ctrl Pts',(3.94611544431017,15.7691023294921,-1.40000000000002));
#10853=CARTESIAN_POINT('Ctrl Pts',(3.84407131175635,15.8322454089585,7.));
#10854=CARTESIAN_POINT('Ctrl Pts',(3.84407131175635,15.8322454089585,-1.40000000000002));
#10855=CARTESIAN_POINT('Ctrl Pts',(3.75315043649997,15.9585748177211,7.));
#10856=CARTESIAN_POINT('Ctrl Pts',(3.75315043649997,15.9585748177211,-1.40000000000002));
#10857=CARTESIAN_POINT('Ctrl Pts',(3.70904952755068,16.0682204478862,7.));
#10858=CARTESIAN_POINT('Ctrl Pts',(3.70904952755068,16.0682204478862,-1.40000000000002));
#10859=CARTESIAN_POINT('Ctrl Pts',(3.68733631276637,16.1718717115691,7.));
#10860=CARTESIAN_POINT('Ctrl Pts',(3.68733631276637,16.1718717115691,-1.40000000000002));
#10861=CARTESIAN_POINT('Ctrl Pts',(3.67963072201293,16.2732984400116,7.));
#10862=CARTESIAN_POINT('Ctrl Pts',(3.67963072201293,16.2732984400116,-1.40000000000002));
#10863=CARTESIAN_POINT('Ctrl Pts',(3.68169968173257,16.3522749650866,7.));
#10864=CARTESIAN_POINT('Ctrl Pts',(3.68169968173257,16.3522749650866,-1.40000000000002));
#10865=CARTESIAN_POINT('Ctrl Pts',(3.68636158229542,16.409563995311,7.));
#10866=CARTESIAN_POINT('Ctrl Pts',(3.68636158229542,16.409563995311,-1.40000000000002));
#10867=CARTESIAN_POINT('Ctrl Pts',(3.69014050504822,16.4450105654964,7.));
#10868=CARTESIAN_POINT('Ctrl Pts',(3.69014050504822,16.4450105654964,-1.40000000000002));
#10869=CARTESIAN_POINT('Ctrl Pts',(3.69552774561756,16.4843881842109,7.));
#10870=CARTESIAN_POINT('Ctrl Pts',(3.69552774561756,16.4843881842109,-1.40000000000002));
#10871=CARTESIAN_POINT('Ctrl Pts',(3.70408422142788,16.5444222357228,7.));
#10872=CARTESIAN_POINT('Ctrl Pts',(3.70408422142788,16.5444222357228,-1.40000000000002));
#10873=CARTESIAN_POINT('Ctrl Pts',(3.71344611165869,16.632533556064,7.));
#10874=CARTESIAN_POINT('Ctrl Pts',(3.71344611165869,16.632533556064,-1.40000000000002));
#10875=CARTESIAN_POINT('Ctrl Pts',(3.72194155665403,16.7524120409277,7.));
#10876=CARTESIAN_POINT('Ctrl Pts',(3.72194155665403,16.7524120409277,-1.40000000000002));
#10877=CARTESIAN_POINT('Ctrl Pts',(3.7266491009471,16.8943723095674,7.));
#10878=CARTESIAN_POINT('Ctrl Pts',(3.7266491009471,16.8943723095674,-1.40000000000002));
#10879=CARTESIAN_POINT('Ctrl Pts',(3.72602328845452,17.0582577813421,7.));
#10880=CARTESIAN_POINT('Ctrl Pts',(3.72602328845452,17.0582577813421,-1.40000000000002));
#10881=CARTESIAN_POINT('Ctrl Pts',(3.71840435546373,17.2438412568379,7.));
#10882=CARTESIAN_POINT('Ctrl Pts',(3.71840435546373,17.2438412568379,-1.40000000000002));
#10883=CARTESIAN_POINT('Ctrl Pts',(3.70218403552947,17.4507975846592,7.));
#10884=CARTESIAN_POINT('Ctrl Pts',(3.70218403552947,17.4507975846592,-1.40000000000002));
#10885=CARTESIAN_POINT('Ctrl Pts',(3.67575622931333,17.6787134541915,7.));
#10886=CARTESIAN_POINT('Ctrl Pts',(3.67575622931333,17.6787134541915,-1.40000000000002));
#10887=CARTESIAN_POINT('Ctrl Pts',(3.63753969769581,17.9270849363835,7.));
#10888=CARTESIAN_POINT('Ctrl Pts',(3.63753969769581,17.9270849363835,-1.40000000000002));
#10889=CARTESIAN_POINT('Ctrl Pts',(3.57255446932205,18.265123941733,7.));
#10890=CARTESIAN_POINT('Ctrl Pts',(3.57255446932205,18.265123941733,-1.40000000000002));
#10891=CARTESIAN_POINT('Ctrl Pts',(3.51033578853423,18.5181384456163,7.));
#10892=CARTESIAN_POINT('Ctrl Pts',(3.51033578853423,18.5181384456163,-1.40000000000002));
#10893=CARTESIAN_POINT('Ctrl Pts',(3.46506965370702,18.6813621637974,7.));
#10894=CARTESIAN_POINT('Ctrl Pts',(3.46506965370702,18.6813621637974,-1.40000000000002));
#10895=CARTESIAN_POINT('',(3.46506965370702,18.6813621637974,7.));
#10896=CARTESIAN_POINT('Origin',(0.,8.67361737988404E-16,7.));
#10897=CARTESIAN_POINT('',(2.47738131311212,18.8377966288375,7.));
#10898=CARTESIAN_POINT('Ctrl Pts',(2.47738131311188,18.8377966288376,7.));
#10899=CARTESIAN_POINT('Ctrl Pts',(2.47738131311188,18.8377966288376,-1.39999999999999));
#10900=CARTESIAN_POINT('Ctrl Pts',(2.38389175781397,18.6965496529788,7.));
#10901=CARTESIAN_POINT('Ctrl Pts',(2.38389175781397,18.6965496529788,-1.39999999999999));
#10902=CARTESIAN_POINT('Ctrl Pts',(2.24653249449213,18.4751451900744,7.));
#10903=CARTESIAN_POINT('Ctrl Pts',(2.24653249449213,18.4751451900744,-1.39999999999999));
#10904=CARTESIAN_POINT('Ctrl Pts',(2.08026807216976,18.1737325312257,7.));
#10905=CARTESIAN_POINT('Ctrl Pts',(2.08026807216976,18.1737325312257,-1.39999999999999));
#10906=CARTESIAN_POINT('Ctrl Pts',(1.96717098182927,17.949326772361,7.));
#10907=CARTESIAN_POINT('Ctrl Pts',(1.96717098182927,17.949326772361,-1.39999999999999));
#10908=CARTESIAN_POINT('Ctrl Pts',(1.87160676754279,17.7407325407201,7.));
#10909=CARTESIAN_POINT('Ctrl Pts',(1.87160676754279,17.7407325407201,-1.39999999999999));
#10910=CARTESIAN_POINT('Ctrl Pts',(1.79222730418274,17.548917731071,7.));
#10911=CARTESIAN_POINT('Ctrl Pts',(1.79222730418274,17.548917731071,-1.39999999999999));
#10912=CARTESIAN_POINT('Ctrl Pts',(1.72763282051121,17.3747717371572,7.));
#10913=CARTESIAN_POINT('Ctrl Pts',(1.72763282051121,17.3747717371572,-1.39999999999999));
#10914=CARTESIAN_POINT('Ctrl Pts',(1.67639424155266,17.2191007779952,7.));
#10915=CARTESIAN_POINT('Ctrl Pts',(1.67639424155266,17.2191007779952,-1.39999999999999));
#10916=CARTESIAN_POINT('Ctrl Pts',(1.63700324669265,17.0826338282621,7.));
#10917=CARTESIAN_POINT('Ctrl Pts',(1.63700324669265,17.0826338282621,-1.39999999999999));
#10918=CARTESIAN_POINT('Ctrl Pts',(1.60803840593148,16.9659973771906,7.));
#10919=CARTESIAN_POINT('Ctrl Pts',(1.60803840593148,16.9659973771906,-1.39999999999999));
#10920=CARTESIAN_POINT('Ctrl Pts',(1.58971419725808,16.8793055486399,7.));
#10921=CARTESIAN_POINT('Ctrl Pts',(1.58971419725808,16.8793055486399,-1.39999999999999));
#10922=CARTESIAN_POINT('Ctrl Pts',(1.57930034717568,16.8195656763126,7.));
#10923=CARTESIAN_POINT('Ctrl Pts',(1.57930034717568,16.8195656763126,-1.39999999999999));
#10924=CARTESIAN_POINT('Ctrl Pts',(1.57225556404314,16.7804505865492,7.));
#10925=CARTESIAN_POINT('Ctrl Pts',(1.57225556404314,16.7804505865492,-1.39999999999999));
#10926=CARTESIAN_POINT('Ctrl Pts',(1.5648959405722,16.7455711436431,7.));
#10927=CARTESIAN_POINT('Ctrl Pts',(1.5648959405722,16.7455711436431,-1.39999999999999));
#10928=CARTESIAN_POINT('Ctrl Pts',(1.5516263875502,16.6896454316358,7.));
#10929=CARTESIAN_POINT('Ctrl Pts',(1.5516263875502,16.6896454316358,-1.39999999999999));
#10930=CARTESIAN_POINT('Ctrl Pts',(1.52918899676866,16.6138949491149,7.));
#10931=CARTESIAN_POINT('Ctrl Pts',(1.52918899676866,16.6138949491149,-1.39999999999999));
#10932=CARTESIAN_POINT('Ctrl Pts',(1.49051796169813,16.5198135565977,7.));
#10933=CARTESIAN_POINT('Ctrl Pts',(1.49051796169813,16.5198135565977,-1.39999999999999));
#10934=CARTESIAN_POINT('Ctrl Pts',(1.43783746532136,16.4279450992207,7.));
#10935=CARTESIAN_POINT('Ctrl Pts',(1.43783746532136,16.4279450992207,-1.39999999999999));
#10936=CARTESIAN_POINT('Ctrl Pts',(1.36201264541063,16.3372938385016,7.));
#10937=CARTESIAN_POINT('Ctrl Pts',(1.36201264541063,16.3372938385016,-1.39999999999999));
#10938=CARTESIAN_POINT('Ctrl Pts',(1.23650382033381,16.2452435266959,7.));
#10939=CARTESIAN_POINT('Ctrl Pts',(1.23650382033381,16.2452435266959,-1.39999999999999));
#10940=CARTESIAN_POINT('Ctrl Pts',(1.11994179848653,16.2167242606458,7.));
#10941=CARTESIAN_POINT('Ctrl Pts',(1.11994179848653,16.2167242606458,-1.39999999999999));
#10942=CARTESIAN_POINT('Ctrl Pts',(1.04967429885989,16.2160625265911,7.));
#10943=CARTESIAN_POINT('Ctrl Pts',(1.04967429885989,16.2160625265911,-1.39999999999999));
#10944=CARTESIAN_POINT('',(1.04967429885989,16.2160625265911,7.));
#10945=CARTESIAN_POINT('Origin',(0.,0.,7.));
#10946=CARTESIAN_POINT('',(-1.04967429885962,16.2160625265911,7.));
#10947=CARTESIAN_POINT('Ctrl Pts',(-1.04967429885986,16.2160625265911,7.));
#10948=CARTESIAN_POINT('Ctrl Pts',(-1.04967429885986,16.2160625265911,-1.4));
#10949=CARTESIAN_POINT('Ctrl Pts',(-1.11994179848651,16.2167242606459,7.));
#10950=CARTESIAN_POINT('Ctrl Pts',(-1.11994179848651,16.2167242606459,-1.4));
#10951=CARTESIAN_POINT('Ctrl Pts',(-1.23650382033378,16.2452435266959,7.));
#10952=CARTESIAN_POINT('Ctrl Pts',(-1.23650382033378,16.2452435266959,-1.4));
#10953=CARTESIAN_POINT('Ctrl Pts',(-1.36201264541058,16.3372938385016,7.));
#10954=CARTESIAN_POINT('Ctrl Pts',(-1.36201264541058,16.3372938385016,-1.4));
#10955=CARTESIAN_POINT('Ctrl Pts',(-1.43783746532133,16.4279450992208,7.));
#10956=CARTESIAN_POINT('Ctrl Pts',(-1.43783746532133,16.4279450992208,-1.4));
#10957=CARTESIAN_POINT('Ctrl Pts',(-1.49051796169812,16.5198135565978,7.));
#10958=CARTESIAN_POINT('Ctrl Pts',(-1.49051796169812,16.5198135565978,-1.4));
#10959=CARTESIAN_POINT('Ctrl Pts',(-1.52918899676864,16.6138949491149,7.));
#10960=CARTESIAN_POINT('Ctrl Pts',(-1.52918899676864,16.6138949491149,-1.4));
#10961=CARTESIAN_POINT('Ctrl Pts',(-1.55162638755018,16.6896454316359,7.));
#10962=CARTESIAN_POINT('Ctrl Pts',(-1.55162638755018,16.6896454316359,-1.4));
#10963=CARTESIAN_POINT('Ctrl Pts',(-1.5648959405722,16.7455711436431,7.));
#10964=CARTESIAN_POINT('Ctrl Pts',(-1.5648959405722,16.7455711436431,-1.4));
#10965=CARTESIAN_POINT('Ctrl Pts',(-1.57225556404314,16.7804505865492,7.));
#10966=CARTESIAN_POINT('Ctrl Pts',(-1.57225556404314,16.7804505865492,-1.4));
#10967=CARTESIAN_POINT('Ctrl Pts',(-1.57930034717564,16.8195656763126,7.));
#10968=CARTESIAN_POINT('Ctrl Pts',(-1.57930034717564,16.8195656763126,-1.4));
#10969=CARTESIAN_POINT('Ctrl Pts',(-1.58971419725806,16.8793055486399,7.));
#10970=CARTESIAN_POINT('Ctrl Pts',(-1.58971419725806,16.8793055486399,-1.4));
#10971=CARTESIAN_POINT('Ctrl Pts',(-1.60803840593146,16.9659973771906,7.));
#10972=CARTESIAN_POINT('Ctrl Pts',(-1.60803840593146,16.9659973771906,-1.4));
#10973=CARTESIAN_POINT('Ctrl Pts',(-1.63700324669262,17.0826338282622,7.));
#10974=CARTESIAN_POINT('Ctrl Pts',(-1.63700324669262,17.0826338282622,-1.4));
#10975=CARTESIAN_POINT('Ctrl Pts',(-1.67639424155265,17.2191007779953,7.));
#10976=CARTESIAN_POINT('Ctrl Pts',(-1.67639424155265,17.2191007779953,-1.4));
#10977=CARTESIAN_POINT('Ctrl Pts',(-1.72763282051122,17.3747717371572,7.));
#10978=CARTESIAN_POINT('Ctrl Pts',(-1.72763282051122,17.3747717371572,-1.4));
#10979=CARTESIAN_POINT('Ctrl Pts',(-1.7922273041827,17.548917731071,7.));
#10980=CARTESIAN_POINT('Ctrl Pts',(-1.7922273041827,17.548917731071,-1.4));
#10981=CARTESIAN_POINT('Ctrl Pts',(-1.87160676754278,17.7407325407201,7.));
#10982=CARTESIAN_POINT('Ctrl Pts',(-1.87160676754278,17.7407325407201,-1.4));
#10983=CARTESIAN_POINT('Ctrl Pts',(-1.96717098182926,17.949326772361,7.));
#10984=CARTESIAN_POINT('Ctrl Pts',(-1.96717098182926,17.949326772361,-1.4));
#10985=CARTESIAN_POINT('Ctrl Pts',(-2.08026807216973,18.1737325312257,7.));
#10986=CARTESIAN_POINT('Ctrl Pts',(-2.08026807216973,18.1737325312257,-1.4));
#10987=CARTESIAN_POINT('Ctrl Pts',(-2.24653249449211,18.4751451900744,7.));
#10988=CARTESIAN_POINT('Ctrl Pts',(-2.24653249449211,18.4751451900744,-1.4));
#10989=CARTESIAN_POINT('Ctrl Pts',(-2.38389175781394,18.6965496529788,7.));
#10990=CARTESIAN_POINT('Ctrl Pts',(-2.38389175781394,18.6965496529788,-1.4));
#10991=CARTESIAN_POINT('Ctrl Pts',(-2.47738131311187,18.8377966288376,7.));
#10992=CARTESIAN_POINT('Ctrl Pts',(-2.47738131311187,18.8377966288376,-1.4));
#10993=CARTESIAN_POINT('',(-2.47738131311187,18.8377966288376,7.));
#10994=CARTESIAN_POINT('Origin',(-1.73472347597681E-15,0.,7.));
#10995=CARTESIAN_POINT('',(-3.46506965370679,18.6813621637974,7.));
#10996=CARTESIAN_POINT('Ctrl Pts',(-3.46506965370701,18.6813621637974,7.));
#10997=CARTESIAN_POINT('Ctrl Pts',(-3.46506965370701,18.6813621637974,-1.39999999999999));
#10998=CARTESIAN_POINT('Ctrl Pts',(-3.51033578853418,18.5181384456162,7.));
#10999=CARTESIAN_POINT('Ctrl Pts',(-3.51033578853418,18.5181384456162,-1.39999999999999));
#11000=CARTESIAN_POINT('Ctrl Pts',(-3.57255446932203,18.265123941733,7.));
#11001=CARTESIAN_POINT('Ctrl Pts',(-3.57255446932203,18.265123941733,-1.39999999999999));
#11002=CARTESIAN_POINT('Ctrl Pts',(-3.63753969769577,17.9270849363835,7.));
#11003=CARTESIAN_POINT('Ctrl Pts',(-3.63753969769577,17.9270849363835,-1.39999999999999));
#11004=CARTESIAN_POINT('Ctrl Pts',(-3.67575622931332,17.6787134541915,7.));
#11005=CARTESIAN_POINT('Ctrl Pts',(-3.67575622931332,17.6787134541915,-1.39999999999999));
#11006=CARTESIAN_POINT('Ctrl Pts',(-3.70218403552948,17.4507975846592,7.));
#11007=CARTESIAN_POINT('Ctrl Pts',(-3.70218403552948,17.4507975846592,-1.39999999999999));
#11008=CARTESIAN_POINT('Ctrl Pts',(-3.7184043554637,17.2438412568379,7.));
#11009=CARTESIAN_POINT('Ctrl Pts',(-3.7184043554637,17.2438412568379,-1.39999999999999));
#11010=CARTESIAN_POINT('Ctrl Pts',(-3.72602328845454,17.0582577813421,7.));
#11011=CARTESIAN_POINT('Ctrl Pts',(-3.72602328845454,17.0582577813421,-1.39999999999999));
#11012=CARTESIAN_POINT('Ctrl Pts',(-3.72664910094709,16.8943723095674,7.));
#11013=CARTESIAN_POINT('Ctrl Pts',(-3.72664910094709,16.8943723095674,-1.39999999999999));
#11014=CARTESIAN_POINT('Ctrl Pts',(-3.72194155665401,16.7524120409277,7.));
#11015=CARTESIAN_POINT('Ctrl Pts',(-3.72194155665401,16.7524120409277,-1.39999999999999));
#11016=CARTESIAN_POINT('Ctrl Pts',(-3.71344611165868,16.632533556064,7.));
#11017=CARTESIAN_POINT('Ctrl Pts',(-3.71344611165868,16.632533556064,-1.39999999999999));
#11018=CARTESIAN_POINT('Ctrl Pts',(-3.70408422142788,16.5444222357228,7.));
#11019=CARTESIAN_POINT('Ctrl Pts',(-3.70408422142788,16.5444222357228,-1.39999999999999));
#11020=CARTESIAN_POINT('Ctrl Pts',(-3.69552774561753,16.4843881842109,7.));
#11021=CARTESIAN_POINT('Ctrl Pts',(-3.69552774561753,16.4843881842109,-1.39999999999999));
#11022=CARTESIAN_POINT('Ctrl Pts',(-3.69014050504823,16.4450105654964,7.));
#11023=CARTESIAN_POINT('Ctrl Pts',(-3.69014050504823,16.4450105654964,-1.39999999999999));
#11024=CARTESIAN_POINT('Ctrl Pts',(-3.68636158229542,16.409563995311,7.));
#11025=CARTESIAN_POINT('Ctrl Pts',(-3.68636158229542,16.409563995311,-1.39999999999999));
#11026=CARTESIAN_POINT('Ctrl Pts',(-3.68169968173256,16.3522749650865,7.));
#11027=CARTESIAN_POINT('Ctrl Pts',(-3.68169968173256,16.3522749650865,-1.39999999999999));
#11028=CARTESIAN_POINT('Ctrl Pts',(-3.67963072201293,16.2732984400115,7.));
#11029=CARTESIAN_POINT('Ctrl Pts',(-3.67963072201293,16.2732984400115,-1.39999999999999));
#11030=CARTESIAN_POINT('Ctrl Pts',(-3.68733631276638,16.1718717115691,7.));
#11031=CARTESIAN_POINT('Ctrl Pts',(-3.68733631276638,16.1718717115691,-1.39999999999999));
#11032=CARTESIAN_POINT('Ctrl Pts',(-3.70904952755066,16.0682204478862,7.));
#11033=CARTESIAN_POINT('Ctrl Pts',(-3.70904952755066,16.0682204478862,-1.39999999999999));
#11034=CARTESIAN_POINT('Ctrl Pts',(-3.75315043649994,15.958574817721,7.));
#11035=CARTESIAN_POINT('Ctrl Pts',(-3.75315043649994,15.958574817721,-1.39999999999999));
#11036=CARTESIAN_POINT('Ctrl Pts',(-3.84407131175633,15.8322454089585,7.));
#11037=CARTESIAN_POINT('Ctrl Pts',(-3.84407131175633,15.8322454089585,-1.39999999999999));
#11038=CARTESIAN_POINT('Ctrl Pts',(-3.94611544431016,15.7691023294921,7.));
#11039=CARTESIAN_POINT('Ctrl Pts',(-3.94611544431016,15.7691023294921,-1.39999999999999));
#11040=CARTESIAN_POINT('Ctrl Pts',(-4.01273932064518,15.7467591314705,7.));
#11041=CARTESIAN_POINT('Ctrl Pts',(-4.01273932064518,15.7467591314705,-1.39999999999999));
#11042=CARTESIAN_POINT('',(-4.01273932064518,15.7467591314705,7.));
#11043=CARTESIAN_POINT('Origin',(0.,0.,7.));
#11044=CARTESIAN_POINT('',(-6.00933848448141,15.0980247376579,7.));
#11045=CARTESIAN_POINT('Ctrl Pts',(-6.00933848448163,15.0980247376578,7.));
#11046=CARTESIAN_POINT('Ctrl Pts',(-6.00933848448163,15.0980247376578,-1.4));
#11047=CARTESIAN_POINT('Ctrl Pts',(-6.076371334954,15.0769402326058,7.));
#11048=CARTESIAN_POINT('Ctrl Pts',(-6.076371334954,15.0769402326058,-1.4));
#11049=CARTESIAN_POINT('Ctrl Pts',(-6.19604134326094,15.0680440207731,7.));
#11050=CARTESIAN_POINT('Ctrl Pts',(-6.19604134326094,15.0680440207731,-1.4));
#11051=CARTESIAN_POINT('Ctrl Pts',(-6.34385243988825,15.1168047097501,7.));
#11052=CARTESIAN_POINT('Ctrl Pts',(-6.34385243988825,15.1168047097501,-1.4));
#11053=CARTESIAN_POINT('Ctrl Pts',(-6.44397890908501,15.1795880240196,7.));
#11054=CARTESIAN_POINT('Ctrl Pts',(-6.44397890908501,15.1795880240196,-1.4));
#11055=CARTESIAN_POINT('Ctrl Pts',(-6.52246995302233,15.2506809503975,7.));
#11056=CARTESIAN_POINT('Ctrl Pts',(-6.52246995302233,15.2506809503975,-1.4));
#11057=CARTESIAN_POINT('Ctrl Pts',(-6.58832104206028,15.3282076647862,7.));
#11058=CARTESIAN_POINT('Ctrl Pts',(-6.58832104206028,15.3282076647862,-1.4));
#11059=CARTESIAN_POINT('Ctrl Pts',(-6.63306845520281,15.3933171197393,7.));
#11060=CARTESIAN_POINT('Ctrl Pts',(-6.63306845520281,15.3933171197393,-1.4));
#11061=CARTESIAN_POINT('Ctrl Pts',(-6.66297054550547,15.4424051151807,7.));
#11062=CARTESIAN_POINT('Ctrl Pts',(-6.66297054550547,15.4424051151807,-1.4));
#11063=CARTESIAN_POINT('Ctrl Pts',(-6.68074830397731,15.4733031879166,7.));
#11064=CARTESIAN_POINT('Ctrl Pts',(-6.68074830397731,15.4733031879166,-1.4));
#11065=CARTESIAN_POINT('Ctrl Pts',(-6.69953551835474,15.5083268912119,7.));
#11066=CARTESIAN_POINT('Ctrl Pts',(-6.69953551835474,15.5083268912119,-1.4));
#11067=CARTESIAN_POINT('Ctrl Pts',(-6.72790031412628,15.5619248294191,7.));
#11068=CARTESIAN_POINT('Ctrl Pts',(-6.72790031412628,15.5619248294191,-1.4));
#11069=CARTESIAN_POINT('Ctrl Pts',(-6.77211692048667,15.6387111659832,7.));
#11070=CARTESIAN_POINT('Ctrl Pts',(-6.77211692048667,15.6387111659832,-1.4));
#11071=CARTESIAN_POINT('Ctrl Pts',(-6.83570676658072,15.7406883947778,7.));
#11072=CARTESIAN_POINT('Ctrl Pts',(-6.83570676658072,15.7406883947778,-1.4));
#11073=CARTESIAN_POINT('Ctrl Pts',(-6.91534043556374,15.8583036897433,7.));
#11074=CARTESIAN_POINT('Ctrl Pts',(-6.91534043556374,15.8583036897433,-1.4));
#11075=CARTESIAN_POINT('Ctrl Pts',(-7.01217619187967,15.9905219781863,7.));
#11076=CARTESIAN_POINT('Ctrl Pts',(-7.01217619187967,15.9905219781863,-1.4));
#11077=CARTESIAN_POINT('Ctrl Pts',(-7.12742326811385,16.1361838672874,7.));
#11078=CARTESIAN_POINT('Ctrl Pts',(-7.12742326811385,16.1361838672874,-1.4));
#11079=CARTESIAN_POINT('Ctrl Pts',(-7.26219165995682,16.2940809887434,7.));
#11080=CARTESIAN_POINT('Ctrl Pts',(-7.26219165995682,16.2940809887434,-1.4));
#11081=CARTESIAN_POINT('Ctrl Pts',(-7.41753779118424,16.4629349257385,7.));
#11082=CARTESIAN_POINT('Ctrl Pts',(-7.41753779118424,16.4629349257385,-1.4));
#11083=CARTESIAN_POINT('Ctrl Pts',(-7.59444470905137,16.6414085620714,7.));
#11084=CARTESIAN_POINT('Ctrl Pts',(-7.59444470905137,16.6414085620714,-1.4));
#11085=CARTESIAN_POINT('Ctrl Pts',(-7.8457132052331,16.8766905033058,7.));
#11086=CARTESIAN_POINT('Ctrl Pts',(-7.8457132052331,16.8766905033058,-1.4));
#11087=CARTESIAN_POINT('Ctrl Pts',(-8.04476736935674,17.0448123137865,7.));
#11088=CARTESIAN_POINT('Ctrl Pts',(-8.04476736935674,17.0448123137865,-1.4));
#11089=CARTESIAN_POINT('Ctrl Pts',(-8.1773289360728,17.1502563092004,7.));
#11090=CARTESIAN_POINT('Ctrl Pts',(-8.1773289360728,17.1502563092004,-1.4));
#11091=CARTESIAN_POINT('',(-8.1773289360728,17.1502563092004,7.));
#11092=CARTESIAN_POINT('Origin',(1.73472347597681E-15,0.,7.));
#11093=CARTESIAN_POINT('',(-9.06833546026097,16.6962658094609,7.));
#11094=CARTESIAN_POINT('Ctrl Pts',(-9.06833546026118,16.6962658094608,7.));
#11095=CARTESIAN_POINT('Ctrl Pts',(-9.06833546026118,16.6962658094608,-1.39999999999999));
#11096=CARTESIAN_POINT('Ctrl Pts',(-9.06094720995302,16.5270428237395,7.));
#11097=CARTESIAN_POINT('Ctrl Pts',(-9.06094720995302,16.5270428237395,-1.39999999999999));
#11098=CARTESIAN_POINT('Ctrl Pts',(-9.04193491022831,16.2671851013731,7.));
#11099=CARTESIAN_POINT('Ctrl Pts',(-9.04193491022831,16.2671851013731,-1.39999999999999));
#11100=CARTESIAN_POINT('Ctrl Pts',(-8.9992797377215,15.9256093626227,7.));
#11101=CARTESIAN_POINT('Ctrl Pts',(-8.9992797377215,15.9256093626227,-1.39999999999999));
#11102=CARTESIAN_POINT('Ctrl Pts',(-8.95887481023115,15.6775844882862,7.));
#11103=CARTESIAN_POINT('Ctrl Pts',(-8.95887481023115,15.6775844882862,-1.39999999999999));
#11104=CARTESIAN_POINT('Ctrl Pts',(-8.91357927057119,15.4526569741556,7.));
#11105=CARTESIAN_POINT('Ctrl Pts',(-8.91357927057119,15.4526569741556,-1.39999999999999));
#11106=CARTESIAN_POINT('Ctrl Pts',(-8.8650526891508,15.2508174554788,7.));
#11107=CARTESIAN_POINT('Ctrl Pts',(-8.8650526891508,15.2508174554788,-1.39999999999999));
#11108=CARTESIAN_POINT('Ctrl Pts',(-8.81495027721559,15.0719627020186,7.));
#11109=CARTESIAN_POINT('Ctrl Pts',(-8.81495027721559,15.0719627020186,-1.39999999999999));
#11110=CARTESIAN_POINT('Ctrl Pts',(-8.76490206435507,14.9159049694657,7.));
#11111=CARTESIAN_POINT('Ctrl Pts',(-8.76490206435507,14.9159049694657,-1.39999999999999));
#11112=CARTESIAN_POINT('Ctrl Pts',(-8.71655678814369,14.7823474421093,7.));
#11113=CARTESIAN_POINT('Ctrl Pts',(-8.71655678814369,14.7823474421093,-1.39999999999999));
#11114=CARTESIAN_POINT('Ctrl Pts',(-8.67143265073926,14.6709614647944,7.));
#11115=CARTESIAN_POINT('Ctrl Pts',(-8.67143265073926,14.6709614647944,-1.39999999999999));
#11116=CARTESIAN_POINT('Ctrl Pts',(-8.63530106864816,14.5900556026053,7.));
#11117=CARTESIAN_POINT('Ctrl Pts',(-8.63530106864816,14.5900556026053,-1.39999999999999));
#11118=CARTESIAN_POINT('Ctrl Pts',(-8.60861183441386,14.5356039231527,7.));
#11119=CARTESIAN_POINT('Ctrl Pts',(-8.60861183441386,14.5356039231527,-1.39999999999999));
#11120=CARTESIAN_POINT('Ctrl Pts',(-8.59131991078476,14.4998183311667,7.));
#11121=CARTESIAN_POINT('Ctrl Pts',(-8.59131991078476,14.4998183311667,-1.39999999999999));
#11122=CARTESIAN_POINT('Ctrl Pts',(-8.57677234909655,14.4672743909627,7.));
#11123=CARTESIAN_POINT('Ctrl Pts',(-8.57677234909655,14.4672743909627,-1.39999999999999));
#11124=CARTESIAN_POINT('Ctrl Pts',(-8.55463533425729,14.4142298919554,7.));
#11125=CARTESIAN_POINT('Ctrl Pts',(-8.55463533425729,14.4142298919554,-1.39999999999999));
#11126=CARTESIAN_POINT('Ctrl Pts',(-8.52826254822913,14.3397580968626,7.));
#11127=CARTESIAN_POINT('Ctrl Pts',(-8.52826254822913,14.3397580968626,-1.39999999999999));
#11128=CARTESIAN_POINT('Ctrl Pts',(-8.50424841775454,14.2409143873564,7.));
#11129=CARTESIAN_POINT('Ctrl Pts',(-8.50424841775454,14.2409143873564,-1.39999999999999));
#11130=CARTESIAN_POINT('Ctrl Pts',(-8.49286891019839,14.1356264252377,7.));
#11131=CARTESIAN_POINT('Ctrl Pts',(-8.49286891019839,14.1356264252377,-1.39999999999999));
#11132=CARTESIAN_POINT('Ctrl Pts',(-8.50092900394916,14.0177193038531,7.));
#11133=CARTESIAN_POINT('Ctrl Pts',(-8.50092900394916,14.0177193038531,-1.39999999999999));
#11134=CARTESIAN_POINT('Ctrl Pts',(-8.54836196063204,13.8694768008521,7.));
#11135=CARTESIAN_POINT('Ctrl Pts',(-8.54836196063204,13.8694768008521,-1.39999999999999));
#11136=CARTESIAN_POINT('Ctrl Pts',(-8.62589941321477,13.7778907925313,7.));
#11137=CARTESIAN_POINT('Ctrl Pts',(-8.62589941321477,13.7778907925313,-1.39999999999999));
#11138=CARTESIAN_POINT('Ctrl Pts',(-8.68235805704666,13.7360532384392,7.));
#11139=CARTESIAN_POINT('Ctrl Pts',(-8.68235805704666,13.7360532384392,-1.39999999999999));
#11140=CARTESIAN_POINT('',(-8.68235805704666,13.7360532384392,7.));
#11141=CARTESIAN_POINT('Origin',(0.,0.,7.));
#11142=CARTESIAN_POINT('',(-10.380766749719,12.5020870932788,7.));
#11143=CARTESIAN_POINT('Ctrl Pts',(-10.3807667497191,12.5020870932787,7.));
#11144=CARTESIAN_POINT('Ctrl Pts',(-10.3807667497191,12.5020870932787,-1.4));
#11145=CARTESIAN_POINT('Ctrl Pts',(-10.4380033085876,12.4613202473787,7.));
#11146=CARTESIAN_POINT('Ctrl Pts',(-10.4380033085876,12.4613202473787,-1.4));
#11147=CARTESIAN_POINT('Ctrl Pts',(-10.5490671691512,12.4158793808611,7.));
#11148=CARTESIAN_POINT('Ctrl Pts',(-10.5490671691512,12.4158793808611,-1.4));
#11149=CARTESIAN_POINT('Ctrl Pts',(-10.7047117573307,12.4165774110367,7.));
#11150=CARTESIAN_POINT('Ctrl Pts',(-10.7047117573307,12.4165774110367,-1.4));
#11151=CARTESIAN_POINT('Ctrl Pts',(-10.8193387993863,12.4453471106187,7.));
#11152=CARTESIAN_POINT('Ctrl Pts',(-10.8193387993863,12.4453471106187,-1.4));
#11153=CARTESIAN_POINT('Ctrl Pts',(-10.9159571406243,12.48870543503,7.));
#11154=CARTESIAN_POINT('Ctrl Pts',(-10.9159571406243,12.48870543503,-1.4));
#11155=CARTESIAN_POINT('Ctrl Pts',(-11.0025423202232,12.5420886163255,7.));
#11156=CARTESIAN_POINT('Ctrl Pts',(-11.0025423202232,12.5420886163255,-1.4));
#11157=CARTESIAN_POINT('Ctrl Pts',(-11.0652195671547,12.5901836766158,7.));
#11158=CARTESIAN_POINT('Ctrl Pts',(-11.0652195671547,12.5901836766158,-1.4));
#11159=CARTESIAN_POINT('Ctrl Pts',(-11.1088271697991,12.6276288804813,7.));
#11160=CARTESIAN_POINT('Ctrl Pts',(-11.1088271697991,12.6276288804813,-1.4));
#11161=CARTESIAN_POINT('Ctrl Pts',(-11.1352828524077,12.651521064408,7.));
#11162=CARTESIAN_POINT('Ctrl Pts',(-11.1352828524077,12.651521064408,-1.4));
#11163=CARTESIAN_POINT('Ctrl Pts',(-11.1639734745886,12.6790250171322,7.));
#11164=CARTESIAN_POINT('Ctrl Pts',(-11.1639734745886,12.6790250171322,-1.4));
#11165=CARTESIAN_POINT('Ctrl Pts',(-11.20751267221,12.7212344815888,7.));
#11166=CARTESIAN_POINT('Ctrl Pts',(-11.20751267221,12.7212344815888,-1.4));
#11167=CARTESIAN_POINT('Ctrl Pts',(-11.2732934467516,12.7805989445416,7.));
#11168=CARTESIAN_POINT('Ctrl Pts',(-11.2732934467516,12.7805989445416,-1.4));
#11169=CARTESIAN_POINT('Ctrl Pts',(-11.3652836809863,12.8579347093876,7.));
#11170=CARTESIAN_POINT('Ctrl Pts',(-11.3652836809863,12.8579347093876,-1.4));
#11171=CARTESIAN_POINT('Ctrl Pts',(-11.4773649257319,12.9451853450404,7.));
#11172=CARTESIAN_POINT('Ctrl Pts',(-11.4773649257319,12.9451853450404,-1.4));
#11173=CARTESIAN_POINT('Ctrl Pts',(-11.6103189008826,13.0410085154727,7.));
#11174=CARTESIAN_POINT('Ctrl Pts',(-11.6103189008826,13.0410085154727,-1.4));
#11175=CARTESIAN_POINT('Ctrl Pts',(-11.764937382884,13.1439278991698,7.));
#11176=CARTESIAN_POINT('Ctrl Pts',(-11.764937382884,13.1439278991698,-1.4));
#11177=CARTESIAN_POINT('Ctrl Pts',(-11.9419026340297,13.2524512620507,7.));
#11178=CARTESIAN_POINT('Ctrl Pts',(-11.9419026340297,13.2524512620507,-1.4));
#11179=CARTESIAN_POINT('Ctrl Pts',(-12.1418243205134,13.3650363045724,7.));
#11180=CARTESIAN_POINT('Ctrl Pts',(-12.1418243205134,13.3650363045724,-1.4));
#11181=CARTESIAN_POINT('Ctrl Pts',(-12.3652241842034,13.4801075753502,7.));
#11182=CARTESIAN_POINT('Ctrl Pts',(-12.3652241842034,13.4801075753502,-1.4));
#11183=CARTESIAN_POINT('Ctrl Pts',(-12.6769008431476,13.6262277632565,7.));
#11184=CARTESIAN_POINT('Ctrl Pts',(-12.6769008431476,13.6262277632565,-1.4));
#11185=CARTESIAN_POINT('Ctrl Pts',(-12.9181650995968,13.7246099871303,7.));
#11186=CARTESIAN_POINT('Ctrl Pts',(-12.9181650995968,13.7246099871303,-1.4));
#11187=CARTESIAN_POINT('Ctrl Pts',(-13.07682262797,13.7839294091566,7.));
#11188=CARTESIAN_POINT('Ctrl Pts',(-13.07682262797,13.7839294091566,-1.4));
#11189=CARTESIAN_POINT('',(-13.07682262797,13.7839294091566,7.));
#11190=CARTESIAN_POINT('Origin',(1.57723797680727E-16,0.,7.));
#11191=CARTESIAN_POINT('',(-13.7839294091564,13.0768226279702,7.));
#11192=CARTESIAN_POINT('Ctrl Pts',(-13.7839294091566,13.07682262797,7.));
#11193=CARTESIAN_POINT('Ctrl Pts',(-13.7839294091566,13.07682262797,-1.39999999999999));
#11194=CARTESIAN_POINT('Ctrl Pts',(-13.7246099871302,12.9181650995968,7.));
#11195=CARTESIAN_POINT('Ctrl Pts',(-13.7246099871302,12.9181650995968,-1.39999999999999));
#11196=CARTESIAN_POINT('Ctrl Pts',(-13.6262277632565,12.6769008431476,7.));
#11197=CARTESIAN_POINT('Ctrl Pts',(-13.6262277632565,12.6769008431476,-1.39999999999999));
#11198=CARTESIAN_POINT('Ctrl Pts',(-13.4801075753502,12.3652241842034,7.));
#11199=CARTESIAN_POINT('Ctrl Pts',(-13.4801075753502,12.3652241842034,-1.39999999999999));
#11200=CARTESIAN_POINT('Ctrl Pts',(-13.3650363045723,12.1418243205134,7.));
#11201=CARTESIAN_POINT('Ctrl Pts',(-13.3650363045723,12.1418243205134,-1.39999999999999));
#11202=CARTESIAN_POINT('Ctrl Pts',(-13.2524512620508,11.9419026340297,7.));
#11203=CARTESIAN_POINT('Ctrl Pts',(-13.2524512620508,11.9419026340297,-1.39999999999999));
#11204=CARTESIAN_POINT('Ctrl Pts',(-13.1439278991698,11.764937382884,7.));
#11205=CARTESIAN_POINT('Ctrl Pts',(-13.1439278991698,11.764937382884,-1.39999999999999));
#11206=CARTESIAN_POINT('Ctrl Pts',(-13.0410085154728,11.6103189008826,7.));
#11207=CARTESIAN_POINT('Ctrl Pts',(-13.0410085154728,11.6103189008826,-1.39999999999999));
#11208=CARTESIAN_POINT('Ctrl Pts',(-12.9451853450404,11.4773649257318,7.));
#11209=CARTESIAN_POINT('Ctrl Pts',(-12.9451853450404,11.4773649257318,-1.39999999999999));
#11210=CARTESIAN_POINT('Ctrl Pts',(-12.8579347093876,11.3652836809863,7.));
#11211=CARTESIAN_POINT('Ctrl Pts',(-12.8579347093876,11.3652836809863,-1.39999999999999));
#11212=CARTESIAN_POINT('Ctrl Pts',(-12.7805989445416,11.2732934467516,7.));
#11213=CARTESIAN_POINT('Ctrl Pts',(-12.7805989445416,11.2732934467516,-1.39999999999999));
#11214=CARTESIAN_POINT('Ctrl Pts',(-12.7212344815888,11.2075126722099,7.));
#11215=CARTESIAN_POINT('Ctrl Pts',(-12.7212344815888,11.2075126722099,-1.39999999999999));
#11216=CARTESIAN_POINT('Ctrl Pts',(-12.6790250171322,11.1639734745886,7.));
#11217=CARTESIAN_POINT('Ctrl Pts',(-12.6790250171322,11.1639734745886,-1.39999999999999));
#11218=CARTESIAN_POINT('Ctrl Pts',(-12.651521064408,11.1352828524077,7.));
#11219=CARTESIAN_POINT('Ctrl Pts',(-12.651521064408,11.1352828524077,-1.39999999999999));
#11220=CARTESIAN_POINT('Ctrl Pts',(-12.6276288804813,11.1088271697991,7.));
#11221=CARTESIAN_POINT('Ctrl Pts',(-12.6276288804813,11.1088271697991,-1.39999999999999));
#11222=CARTESIAN_POINT('Ctrl Pts',(-12.5901836766158,11.0652195671547,7.));
#11223=CARTESIAN_POINT('Ctrl Pts',(-12.5901836766158,11.0652195671547,-1.39999999999999));
#11224=CARTESIAN_POINT('Ctrl Pts',(-12.5420886163255,11.0025423202231,7.));
#11225=CARTESIAN_POINT('Ctrl Pts',(-12.5420886163255,11.0025423202231,-1.39999999999999));
#11226=CARTESIAN_POINT('Ctrl Pts',(-12.48870543503,10.9159571406243,7.));
#11227=CARTESIAN_POINT('Ctrl Pts',(-12.48870543503,10.9159571406243,-1.39999999999999));
#11228=CARTESIAN_POINT('Ctrl Pts',(-12.4453471106187,10.8193387993863,7.));
#11229=CARTESIAN_POINT('Ctrl Pts',(-12.4453471106187,10.8193387993863,-1.39999999999999));
#11230=CARTESIAN_POINT('Ctrl Pts',(-12.4165774110367,10.7047117573307,7.));
#11231=CARTESIAN_POINT('Ctrl Pts',(-12.4165774110367,10.7047117573307,-1.39999999999999));
#11232=CARTESIAN_POINT('Ctrl Pts',(-12.4158793808611,10.5490671691512,7.));
#11233=CARTESIAN_POINT('Ctrl Pts',(-12.4158793808611,10.5490671691512,-1.39999999999999));
#11234=CARTESIAN_POINT('Ctrl Pts',(-12.4613202473787,10.4380033085876,7.));
#11235=CARTESIAN_POINT('Ctrl Pts',(-12.4613202473787,10.4380033085876,-1.39999999999999));
#11236=CARTESIAN_POINT('Ctrl Pts',(-12.5020870932787,10.3807667497191,7.));
#11237=CARTESIAN_POINT('Ctrl Pts',(-12.5020870932787,10.3807667497191,-1.39999999999999));
#11238=CARTESIAN_POINT('',(-12.5020870932787,10.3807667497191,7.));
#11239=CARTESIAN_POINT('Origin',(0.,0.,7.));
#11240=CARTESIAN_POINT('',(-13.7360532384391,8.68235805704682,7.));
#11241=CARTESIAN_POINT('Ctrl Pts',(-13.7360532384392,8.68235805704666,7.));
#11242=CARTESIAN_POINT('Ctrl Pts',(-13.7360532384392,8.68235805704666,-1.4));
#11243=CARTESIAN_POINT('Ctrl Pts',(-13.7778907925313,8.62589941321479,7.));
#11244=CARTESIAN_POINT('Ctrl Pts',(-13.7778907925313,8.62589941321479,-1.4));
#11245=CARTESIAN_POINT('Ctrl Pts',(-13.8694768008521,8.54836196063206,7.));
#11246=CARTESIAN_POINT('Ctrl Pts',(-13.8694768008521,8.54836196063206,-1.4));
#11247=CARTESIAN_POINT('Ctrl Pts',(-14.0177193038531,8.50092900394919,7.));
#11248=CARTESIAN_POINT('Ctrl Pts',(-14.0177193038531,8.50092900394919,-1.4));
#11249=CARTESIAN_POINT('Ctrl Pts',(-14.1356264252377,8.49286891019842,7.));
#11250=CARTESIAN_POINT('Ctrl Pts',(-14.1356264252377,8.49286891019842,-1.4));
#11251=CARTESIAN_POINT('Ctrl Pts',(-14.2409143873564,8.50424841775455,7.));
#11252=CARTESIAN_POINT('Ctrl Pts',(-14.2409143873564,8.50424841775455,-1.4));
#11253=CARTESIAN_POINT('Ctrl Pts',(-14.3397580968626,8.52826254822914,7.));
#11254=CARTESIAN_POINT('Ctrl Pts',(-14.3397580968626,8.52826254822914,-1.4));
#11255=CARTESIAN_POINT('Ctrl Pts',(-14.4142298919555,8.55463533425731,7.));
#11256=CARTESIAN_POINT('Ctrl Pts',(-14.4142298919555,8.55463533425731,-1.4));
#11257=CARTESIAN_POINT('Ctrl Pts',(-14.4672743909627,8.57677234909655,7.));
#11258=CARTESIAN_POINT('Ctrl Pts',(-14.4672743909627,8.57677234909655,-1.4));
#11259=CARTESIAN_POINT('Ctrl Pts',(-14.4998183311667,8.59131991078475,7.));
#11260=CARTESIAN_POINT('Ctrl Pts',(-14.4998183311667,8.59131991078475,-1.4));
#11261=CARTESIAN_POINT('Ctrl Pts',(-14.5356039231527,8.60861183441388,7.));
#11262=CARTESIAN_POINT('Ctrl Pts',(-14.5356039231527,8.60861183441388,-1.4));
#11263=CARTESIAN_POINT('Ctrl Pts',(-14.5900556026053,8.63530106864817,7.));
#11264=CARTESIAN_POINT('Ctrl Pts',(-14.5900556026053,8.63530106864817,-1.4));
#11265=CARTESIAN_POINT('Ctrl Pts',(-14.6709614647944,8.67143265073926,7.));
#11266=CARTESIAN_POINT('Ctrl Pts',(-14.6709614647944,8.67143265073926,-1.4));
#11267=CARTESIAN_POINT('Ctrl Pts',(-14.7823474421093,8.71655678814371,7.));
#11268=CARTESIAN_POINT('Ctrl Pts',(-14.7823474421093,8.71655678814371,-1.4));
#11269=CARTESIAN_POINT('Ctrl Pts',(-14.9159049694657,8.76490206435508,7.));
#11270=CARTESIAN_POINT('Ctrl Pts',(-14.9159049694657,8.76490206435508,-1.4));
#11271=CARTESIAN_POINT('Ctrl Pts',(-15.0719627020186,8.81495027721556,7.));
#11272=CARTESIAN_POINT('Ctrl Pts',(-15.0719627020186,8.81495027721556,-1.4));
#11273=CARTESIAN_POINT('Ctrl Pts',(-15.2508174554788,8.86505268915083,7.));
#11274=CARTESIAN_POINT('Ctrl Pts',(-15.2508174554788,8.86505268915083,-1.4));
#11275=CARTESIAN_POINT('Ctrl Pts',(-15.4526569741556,8.91357927057117,7.));
#11276=CARTESIAN_POINT('Ctrl Pts',(-15.4526569741556,8.91357927057117,-1.4));
#11277=CARTESIAN_POINT('Ctrl Pts',(-15.6775844882863,8.95887481023116,7.));
#11278=CARTESIAN_POINT('Ctrl Pts',(-15.6775844882863,8.95887481023116,-1.4));
#11279=CARTESIAN_POINT('Ctrl Pts',(-15.9256093626227,8.99927973772153,7.));
#11280=CARTESIAN_POINT('Ctrl Pts',(-15.9256093626227,8.99927973772153,-1.4));
#11281=CARTESIAN_POINT('Ctrl Pts',(-16.2671851013731,9.04193491022832,7.));
#11282=CARTESIAN_POINT('Ctrl Pts',(-16.2671851013731,9.04193491022832,-1.4));
#11283=CARTESIAN_POINT('Ctrl Pts',(-16.5270428237395,9.06094720995306,7.));
#11284=CARTESIAN_POINT('Ctrl Pts',(-16.5270428237395,9.06094720995306,-1.4));
#11285=CARTESIAN_POINT('Ctrl Pts',(-16.6962658094608,9.06833546026117,7.));
#11286=CARTESIAN_POINT('Ctrl Pts',(-16.6962658094608,9.06833546026117,-1.4));
#11287=CARTESIAN_POINT('',(-16.6962658094608,9.06833546026117,7.));
#11288=CARTESIAN_POINT('Origin',(-1.73472347597681E-15,0.,7.));
#11289=CARTESIAN_POINT('',(-17.1502563092003,8.17732893607296,7.));
#11290=CARTESIAN_POINT('Ctrl Pts',(-17.1502563092004,8.17732893607281,7.));
#11291=CARTESIAN_POINT('Ctrl Pts',(-17.1502563092004,8.17732893607281,-1.39999999999999));
#11292=CARTESIAN_POINT('Ctrl Pts',(-17.0448123137865,8.04476736935675,7.));
#11293=CARTESIAN_POINT('Ctrl Pts',(-17.0448123137865,8.04476736935675,-1.39999999999999));
#11294=CARTESIAN_POINT('Ctrl Pts',(-16.8766905033057,7.8457132052331,7.));
#11295=CARTESIAN_POINT('Ctrl Pts',(-16.8766905033057,7.8457132052331,-1.39999999999999));
#11296=CARTESIAN_POINT('Ctrl Pts',(-16.6414085620714,7.59444470905138,7.));
#11297=CARTESIAN_POINT('Ctrl Pts',(-16.6414085620714,7.59444470905138,-1.39999999999999));
#11298=CARTESIAN_POINT('Ctrl Pts',(-16.4629349257385,7.41753779118423,7.));
#11299=CARTESIAN_POINT('Ctrl Pts',(-16.4629349257385,7.41753779118423,-1.39999999999999));
#11300=CARTESIAN_POINT('Ctrl Pts',(-16.2940809887434,7.26219165995682,7.));
#11301=CARTESIAN_POINT('Ctrl Pts',(-16.2940809887434,7.26219165995682,-1.39999999999999));
#11302=CARTESIAN_POINT('Ctrl Pts',(-16.1361838672874,7.12742326811386,7.));
#11303=CARTESIAN_POINT('Ctrl Pts',(-16.1361838672874,7.12742326811386,-1.39999999999999));
#11304=CARTESIAN_POINT('Ctrl Pts',(-15.9905219781863,7.01217619187965,7.));
#11305=CARTESIAN_POINT('Ctrl Pts',(-15.9905219781863,7.01217619187965,-1.39999999999999));
#11306=CARTESIAN_POINT('Ctrl Pts',(-15.8583036897432,6.91534043556372,7.));
#11307=CARTESIAN_POINT('Ctrl Pts',(-15.8583036897432,6.91534043556372,-1.39999999999999));
#11308=CARTESIAN_POINT('Ctrl Pts',(-15.7406883947777,6.83570676658073,7.));
#11309=CARTESIAN_POINT('Ctrl Pts',(-15.7406883947777,6.83570676658073,-1.39999999999999));
#11310=CARTESIAN_POINT('Ctrl Pts',(-15.6387111659832,6.77211692048666,7.));
#11311=CARTESIAN_POINT('Ctrl Pts',(-15.6387111659832,6.77211692048666,-1.39999999999999));
#11312=CARTESIAN_POINT('Ctrl Pts',(-15.5619248294191,6.72790031412627,7.));
#11313=CARTESIAN_POINT('Ctrl Pts',(-15.5619248294191,6.72790031412627,-1.39999999999999));
#11314=CARTESIAN_POINT('Ctrl Pts',(-15.5083268912118,6.69953551835476,7.));
#11315=CARTESIAN_POINT('Ctrl Pts',(-15.5083268912118,6.69953551835476,-1.39999999999999));
#11316=CARTESIAN_POINT('Ctrl Pts',(-15.4733031879166,6.68074830397729,7.));
#11317=CARTESIAN_POINT('Ctrl Pts',(-15.4733031879166,6.68074830397729,-1.39999999999999));
#11318=CARTESIAN_POINT('Ctrl Pts',(-15.4424051151807,6.66297054550545,7.));
#11319=CARTESIAN_POINT('Ctrl Pts',(-15.4424051151807,6.66297054550545,-1.39999999999999));
#11320=CARTESIAN_POINT('Ctrl Pts',(-15.3933171197393,6.6330684552028,7.));
#11321=CARTESIAN_POINT('Ctrl Pts',(-15.3933171197393,6.6330684552028,-1.39999999999999));
#11322=CARTESIAN_POINT('Ctrl Pts',(-15.3282076647861,6.58832104206026,7.));
#11323=CARTESIAN_POINT('Ctrl Pts',(-15.3282076647861,6.58832104206026,-1.39999999999999));
#11324=CARTESIAN_POINT('Ctrl Pts',(-15.2506809503975,6.5224699530223,7.));
#11325=CARTESIAN_POINT('Ctrl Pts',(-15.2506809503975,6.5224699530223,-1.39999999999999));
#11326=CARTESIAN_POINT('Ctrl Pts',(-15.1795880240196,6.443978909085,7.));
#11327=CARTESIAN_POINT('Ctrl Pts',(-15.1795880240196,6.443978909085,-1.39999999999999));
#11328=CARTESIAN_POINT('Ctrl Pts',(-15.1168047097501,6.34385243988827,7.));
#11329=CARTESIAN_POINT('Ctrl Pts',(-15.1168047097501,6.34385243988827,-1.39999999999999));
#11330=CARTESIAN_POINT('Ctrl Pts',(-15.0680440207731,6.19604134326095,7.));
#11331=CARTESIAN_POINT('Ctrl Pts',(-15.0680440207731,6.19604134326095,-1.39999999999999));
#11332=CARTESIAN_POINT('Ctrl Pts',(-15.0769402326058,6.07637133495398,7.));
#11333=CARTESIAN_POINT('Ctrl Pts',(-15.0769402326058,6.07637133495398,-1.39999999999999));
#11334=CARTESIAN_POINT('Ctrl Pts',(-15.0980247376578,6.00933848448163,7.));
#11335=CARTESIAN_POINT('Ctrl Pts',(-15.0980247376578,6.00933848448163,-1.39999999999999));
#11336=CARTESIAN_POINT('',(-15.0980247376578,6.00933848448163,7.));
#11337=CARTESIAN_POINT('Origin',(0.,0.,7.));
#11338=CARTESIAN_POINT('',(-15.7467591314704,4.01273932064536,7.));
#11339=CARTESIAN_POINT('Ctrl Pts',(-15.7467591314704,4.0127393206452,7.));
#11340=CARTESIAN_POINT('Ctrl Pts',(-15.7467591314704,4.0127393206452,-1.4));
#11341=CARTESIAN_POINT('Ctrl Pts',(-15.7691023294921,3.94611544431018,7.));
#11342=CARTESIAN_POINT('Ctrl Pts',(-15.7691023294921,3.94611544431018,-1.4));
#11343=CARTESIAN_POINT('Ctrl Pts',(-15.8322454089585,3.84407131175636,7.));
#11344=CARTESIAN_POINT('Ctrl Pts',(-15.8322454089585,3.84407131175636,-1.4));
#11345=CARTESIAN_POINT('Ctrl Pts',(-15.958574817721,3.75315043649999,7.));
#11346=CARTESIAN_POINT('Ctrl Pts',(-15.958574817721,3.75315043649999,-1.4));
#11347=CARTESIAN_POINT('Ctrl Pts',(-16.0682204478862,3.7090495275507,7.));
#11348=CARTESIAN_POINT('Ctrl Pts',(-16.0682204478862,3.7090495275507,-1.4));
#11349=CARTESIAN_POINT('Ctrl Pts',(-16.1718717115691,3.68733631276638,7.));
#11350=CARTESIAN_POINT('Ctrl Pts',(-16.1718717115691,3.68733631276638,-1.4));
#11351=CARTESIAN_POINT('Ctrl Pts',(-16.2732984400115,3.67963072201295,7.));
#11352=CARTESIAN_POINT('Ctrl Pts',(-16.2732984400115,3.67963072201295,-1.4));
#11353=CARTESIAN_POINT('Ctrl Pts',(-16.3522749650865,3.68169968173258,7.));
#11354=CARTESIAN_POINT('Ctrl Pts',(-16.3522749650865,3.68169968173258,-1.4));
#11355=CARTESIAN_POINT('Ctrl Pts',(-16.409563995311,3.68636158229543,7.));
#11356=CARTESIAN_POINT('Ctrl Pts',(-16.409563995311,3.68636158229543,-1.4));
#11357=CARTESIAN_POINT('Ctrl Pts',(-16.4450105654964,3.69014050504823,7.));
#11358=CARTESIAN_POINT('Ctrl Pts',(-16.4450105654964,3.69014050504823,-1.4));
#11359=CARTESIAN_POINT('Ctrl Pts',(-16.4843881842109,3.69552774561757,7.));
#11360=CARTESIAN_POINT('Ctrl Pts',(-16.4843881842109,3.69552774561757,-1.4));
#11361=CARTESIAN_POINT('Ctrl Pts',(-16.5444222357228,3.70408422142789,7.));
#11362=CARTESIAN_POINT('Ctrl Pts',(-16.5444222357228,3.70408422142789,-1.4));
#11363=CARTESIAN_POINT('Ctrl Pts',(-16.632533556064,3.7134461116587,7.));
#11364=CARTESIAN_POINT('Ctrl Pts',(-16.632533556064,3.7134461116587,-1.4));
#11365=CARTESIAN_POINT('Ctrl Pts',(-16.7524120409277,3.72194155665404,7.));
#11366=CARTESIAN_POINT('Ctrl Pts',(-16.7524120409277,3.72194155665404,-1.4));
#11367=CARTESIAN_POINT('Ctrl Pts',(-16.8943723095674,3.72664910094711,7.));
#11368=CARTESIAN_POINT('Ctrl Pts',(-16.8943723095674,3.72664910094711,-1.4));
#11369=CARTESIAN_POINT('Ctrl Pts',(-17.0582577813421,3.72602328845453,7.));
#11370=CARTESIAN_POINT('Ctrl Pts',(-17.0582577813421,3.72602328845453,-1.4));
#11371=CARTESIAN_POINT('Ctrl Pts',(-17.2438412568379,3.71840435546374,7.));
#11372=CARTESIAN_POINT('Ctrl Pts',(-17.2438412568379,3.71840435546374,-1.4));
#11373=CARTESIAN_POINT('Ctrl Pts',(-17.4507975846592,3.70218403552947,7.));
#11374=CARTESIAN_POINT('Ctrl Pts',(-17.4507975846592,3.70218403552947,-1.4));
#11375=CARTESIAN_POINT('Ctrl Pts',(-17.6787134541915,3.67575622931334,7.));
#11376=CARTESIAN_POINT('Ctrl Pts',(-17.6787134541915,3.67575622931334,-1.4));
#11377=CARTESIAN_POINT('Ctrl Pts',(-17.9270849363835,3.63753969769581,7.));
#11378=CARTESIAN_POINT('Ctrl Pts',(-17.9270849363835,3.63753969769581,-1.4));
#11379=CARTESIAN_POINT('Ctrl Pts',(-18.265123941733,3.57255446932205,7.));
#11380=CARTESIAN_POINT('Ctrl Pts',(-18.265123941733,3.57255446932205,-1.4));
#11381=CARTESIAN_POINT('Ctrl Pts',(-18.5181384456163,3.51033578853423,7.));
#11382=CARTESIAN_POINT('Ctrl Pts',(-18.5181384456163,3.51033578853423,-1.4));
#11383=CARTESIAN_POINT('Ctrl Pts',(-18.6813621637973,3.46506965370702,7.));
#11384=CARTESIAN_POINT('Ctrl Pts',(-18.6813621637973,3.46506965370702,-1.4));
#11385=CARTESIAN_POINT('',(-18.6813621637973,3.46506965370702,7.));
#11386=CARTESIAN_POINT('Origin',(0.,0.,7.));
#11387=CARTESIAN_POINT('',(-18.8377966288375,2.47738131311205,7.));
#11388=CARTESIAN_POINT('Ctrl Pts',(-18.8377966288376,2.47738131311188,7.));
#11389=CARTESIAN_POINT('Ctrl Pts',(-18.8377966288376,2.47738131311188,-1.39999999999999));
#11390=CARTESIAN_POINT('Ctrl Pts',(-18.6965496529788,2.38389175781397,7.));
#11391=CARTESIAN_POINT('Ctrl Pts',(-18.6965496529788,2.38389175781397,-1.39999999999999));
#11392=CARTESIAN_POINT('Ctrl Pts',(-18.4751451900744,2.24653249449212,7.));
#11393=CARTESIAN_POINT('Ctrl Pts',(-18.4751451900744,2.24653249449212,-1.39999999999999));
#11394=CARTESIAN_POINT('Ctrl Pts',(-18.1737325312257,2.08026807216975,7.));
#11395=CARTESIAN_POINT('Ctrl Pts',(-18.1737325312257,2.08026807216975,-1.39999999999999));
#11396=CARTESIAN_POINT('Ctrl Pts',(-17.949326772361,1.96717098182926,7.));
#11397=CARTESIAN_POINT('Ctrl Pts',(-17.949326772361,1.96717098182926,-1.39999999999999));
#11398=CARTESIAN_POINT('Ctrl Pts',(-17.7407325407201,1.87160676754277,7.));
#11399=CARTESIAN_POINT('Ctrl Pts',(-17.7407325407201,1.87160676754277,-1.39999999999999));
#11400=CARTESIAN_POINT('Ctrl Pts',(-17.548917731071,1.79222730418272,7.));
#11401=CARTESIAN_POINT('Ctrl Pts',(-17.548917731071,1.79222730418272,-1.39999999999999));
#11402=CARTESIAN_POINT('Ctrl Pts',(-17.3747717371572,1.72763282051119,7.));
#11403=CARTESIAN_POINT('Ctrl Pts',(-17.3747717371572,1.72763282051119,-1.39999999999999));
#11404=CARTESIAN_POINT('Ctrl Pts',(-17.2191007779952,1.67639424155264,7.));
#11405=CARTESIAN_POINT('Ctrl Pts',(-17.2191007779952,1.67639424155264,-1.39999999999999));
#11406=CARTESIAN_POINT('Ctrl Pts',(-17.0826338282621,1.63700324669263,7.));
#11407=CARTESIAN_POINT('Ctrl Pts',(-17.0826338282621,1.63700324669263,-1.39999999999999));
#11408=CARTESIAN_POINT('Ctrl Pts',(-16.9659973771906,1.60803840593145,7.));
#11409=CARTESIAN_POINT('Ctrl Pts',(-16.9659973771906,1.60803840593145,-1.39999999999999));
#11410=CARTESIAN_POINT('Ctrl Pts',(-16.8793055486399,1.58971419725805,7.));
#11411=CARTESIAN_POINT('Ctrl Pts',(-16.8793055486399,1.58971419725805,-1.39999999999999));
#11412=CARTESIAN_POINT('Ctrl Pts',(-16.8195656763126,1.57930034717566,7.));
#11413=CARTESIAN_POINT('Ctrl Pts',(-16.8195656763126,1.57930034717566,-1.39999999999999));
#11414=CARTESIAN_POINT('Ctrl Pts',(-16.7804505865492,1.57225556404312,7.));
#11415=CARTESIAN_POINT('Ctrl Pts',(-16.7804505865492,1.57225556404312,-1.39999999999999));
#11416=CARTESIAN_POINT('Ctrl Pts',(-16.7455711436431,1.56489594057218,7.));
#11417=CARTESIAN_POINT('Ctrl Pts',(-16.7455711436431,1.56489594057218,-1.39999999999999));
#11418=CARTESIAN_POINT('Ctrl Pts',(-16.6896454316358,1.55162638755017,7.));
#11419=CARTESIAN_POINT('Ctrl Pts',(-16.6896454316358,1.55162638755017,-1.39999999999999));
#11420=CARTESIAN_POINT('Ctrl Pts',(-16.6138949491149,1.52918899676863,7.));
#11421=CARTESIAN_POINT('Ctrl Pts',(-16.6138949491149,1.52918899676863,-1.39999999999999));
#11422=CARTESIAN_POINT('Ctrl Pts',(-16.5198135565977,1.4905179616981,7.));
#11423=CARTESIAN_POINT('Ctrl Pts',(-16.5198135565977,1.4905179616981,-1.39999999999999));
#11424=CARTESIAN_POINT('Ctrl Pts',(-16.4279450992207,1.43783746532133,7.));
#11425=CARTESIAN_POINT('Ctrl Pts',(-16.4279450992207,1.43783746532133,-1.39999999999999));
#11426=CARTESIAN_POINT('Ctrl Pts',(-16.3372938385016,1.3620126454106,7.));
#11427=CARTESIAN_POINT('Ctrl Pts',(-16.3372938385016,1.3620126454106,-1.39999999999999));
#11428=CARTESIAN_POINT('Ctrl Pts',(-16.2452435266959,1.23650382033378,7.));
#11429=CARTESIAN_POINT('Ctrl Pts',(-16.2452435266959,1.23650382033378,-1.39999999999999));
#11430=CARTESIAN_POINT('Ctrl Pts',(-16.2167242606458,1.1199417984865,7.));
#11431=CARTESIAN_POINT('Ctrl Pts',(-16.2167242606458,1.1199417984865,-1.39999999999999));
#11432=CARTESIAN_POINT('Ctrl Pts',(-16.2160625265911,1.04967429885986,7.));
#11433=CARTESIAN_POINT('Ctrl Pts',(-16.2160625265911,1.04967429885986,-1.39999999999999));
#11434=CARTESIAN_POINT('Ctrl Pts',(-16.2160625265911,-1.04967429885984,
7.));
#11435=CARTESIAN_POINT('Ctrl Pts',(-16.2160625265911,-1.04967429885984,
-1.4));
#11436=CARTESIAN_POINT('Ctrl Pts',(-16.2167242606459,-1.11994179848649,
7.));
#11437=CARTESIAN_POINT('Ctrl Pts',(-16.2167242606459,-1.11994179848649,
-1.4));
#11438=CARTESIAN_POINT('Ctrl Pts',(-16.2452435266959,-1.23650382033376,
7.));
#11439=CARTESIAN_POINT('Ctrl Pts',(-16.2452435266959,-1.23650382033376,
-1.4));
#11440=CARTESIAN_POINT('Ctrl Pts',(-16.3372938385016,-1.36201264541056,
7.));
#11441=CARTESIAN_POINT('Ctrl Pts',(-16.3372938385016,-1.36201264541056,
-1.4));
#11442=CARTESIAN_POINT('Ctrl Pts',(-16.4279450992208,-1.43783746532131,
7.));
#11443=CARTESIAN_POINT('Ctrl Pts',(-16.4279450992208,-1.43783746532131,
-1.4));
#11444=CARTESIAN_POINT('Ctrl Pts',(-16.5198135565978,-1.49051796169811,
7.));
#11445=CARTESIAN_POINT('Ctrl Pts',(-16.5198135565978,-1.49051796169811,
-1.4));
#11446=CARTESIAN_POINT('Ctrl Pts',(-16.6138949491149,-1.52918899676863,
7.));
#11447=CARTESIAN_POINT('Ctrl Pts',(-16.6138949491149,-1.52918899676863,
-1.4));
#11448=CARTESIAN_POINT('Ctrl Pts',(-16.6896454316359,-1.55162638755017,
7.));
#11449=CARTESIAN_POINT('Ctrl Pts',(-16.6896454316359,-1.55162638755017,
-1.4));
#11450=CARTESIAN_POINT('Ctrl Pts',(-16.7455711436431,-1.56489594057219,
7.));
#11451=CARTESIAN_POINT('Ctrl Pts',(-16.7455711436431,-1.56489594057219,
-1.4));
#11452=CARTESIAN_POINT('Ctrl Pts',(-16.7804505865492,-1.57225556404312,
7.));
#11453=CARTESIAN_POINT('Ctrl Pts',(-16.7804505865492,-1.57225556404312,
-1.4));
#11454=CARTESIAN_POINT('Ctrl Pts',(-16.8195656763126,-1.57930034717562,
7.));
#11455=CARTESIAN_POINT('Ctrl Pts',(-16.8195656763126,-1.57930034717562,
-1.4));
#11456=CARTESIAN_POINT('Ctrl Pts',(-16.8793055486399,-1.58971419725805,
7.));
#11457=CARTESIAN_POINT('Ctrl Pts',(-16.8793055486399,-1.58971419725805,
-1.4));
#11458=CARTESIAN_POINT('Ctrl Pts',(-16.9659973771906,-1.60803840593145,
7.));
#11459=CARTESIAN_POINT('Ctrl Pts',(-16.9659973771906,-1.60803840593145,
-1.4));
#11460=CARTESIAN_POINT('Ctrl Pts',(-17.0826338282621,-1.63700324669261,
7.));
#11461=CARTESIAN_POINT('Ctrl Pts',(-17.0826338282621,-1.63700324669261,
-1.4));
#11462=CARTESIAN_POINT('Ctrl Pts',(-17.2191007779953,-1.67639424155264,
7.));
#11463=CARTESIAN_POINT('Ctrl Pts',(-17.2191007779953,-1.67639424155264,
-1.4));
#11464=CARTESIAN_POINT('Ctrl Pts',(-17.3747717371572,-1.72763282051121,
7.));
#11465=CARTESIAN_POINT('Ctrl Pts',(-17.3747717371572,-1.72763282051121,
-1.4));
#11466=CARTESIAN_POINT('Ctrl Pts',(-17.548917731071,-1.79222730418269,7.));
#11467=CARTESIAN_POINT('Ctrl Pts',(-17.548917731071,-1.79222730418269,-1.4));
#11468=CARTESIAN_POINT('Ctrl Pts',(-17.7407325407201,-1.87160676754278,
7.));
#11469=CARTESIAN_POINT('Ctrl Pts',(-17.7407325407201,-1.87160676754278,
-1.4));
#11470=CARTESIAN_POINT('Ctrl Pts',(-17.949326772361,-1.96717098182925,7.));
#11471=CARTESIAN_POINT('Ctrl Pts',(-17.949326772361,-1.96717098182925,-1.4));
#11472=CARTESIAN_POINT('Ctrl Pts',(-18.1737325312258,-2.08026807216972,
7.));
#11473=CARTESIAN_POINT('Ctrl Pts',(-18.1737325312258,-2.08026807216972,
-1.4));
#11474=CARTESIAN_POINT('Ctrl Pts',(-18.4751451900744,-2.2465324944921,7.));
#11475=CARTESIAN_POINT('Ctrl Pts',(-18.4751451900744,-2.2465324944921,-1.4));
#11476=CARTESIAN_POINT('Ctrl Pts',(-18.6965496529788,-2.38389175781394,
7.));
#11477=CARTESIAN_POINT('Ctrl Pts',(-18.6965496529788,-2.38389175781394,
-1.4));
#11478=CARTESIAN_POINT('Ctrl Pts',(-18.8377966288376,-2.47738131311187,
7.));
#11479=CARTESIAN_POINT('Ctrl Pts',(-18.8377966288376,-2.47738131311187,
-1.4));
#11480=CARTESIAN_POINT('',(-18.8377966288376,-2.47738131311187,7.));
#11481=CARTESIAN_POINT('Origin',(0.,0.,7.));
#11482=CARTESIAN_POINT('',(-18.6813621637974,-3.46506965370684,7.));
#11483=CARTESIAN_POINT('Ctrl Pts',(-18.6813621637974,-3.46506965370701,
7.));
#11484=CARTESIAN_POINT('Ctrl Pts',(-18.6813621637974,-3.46506965370701,
-1.39999999999999));
#11485=CARTESIAN_POINT('Ctrl Pts',(-18.5181384456162,-3.51033578853419,
7.));
#11486=CARTESIAN_POINT('Ctrl Pts',(-18.5181384456162,-3.51033578853419,
-1.39999999999999));
#11487=CARTESIAN_POINT('Ctrl Pts',(-18.265123941733,-3.57255446932203,7.));
#11488=CARTESIAN_POINT('Ctrl Pts',(-18.265123941733,-3.57255446932203,-1.39999999999999));
#11489=CARTESIAN_POINT('Ctrl Pts',(-17.9270849363835,-3.63753969769578,
7.));
#11490=CARTESIAN_POINT('Ctrl Pts',(-17.9270849363835,-3.63753969769578,
-1.39999999999999));
#11491=CARTESIAN_POINT('Ctrl Pts',(-17.6787134541915,-3.67575622931333,
7.));
#11492=CARTESIAN_POINT('Ctrl Pts',(-17.6787134541915,-3.67575622931333,
-1.39999999999999));
#11493=CARTESIAN_POINT('Ctrl Pts',(-17.4507975846592,-3.70218403552949,
7.));
#11494=CARTESIAN_POINT('Ctrl Pts',(-17.4507975846592,-3.70218403552949,
-1.39999999999999));
#11495=CARTESIAN_POINT('Ctrl Pts',(-17.2438412568379,-3.71840435546371,
7.));
#11496=CARTESIAN_POINT('Ctrl Pts',(-17.2438412568379,-3.71840435546371,
-1.39999999999999));
#11497=CARTESIAN_POINT('Ctrl Pts',(-17.0582577813421,-3.72602328845455,
7.));
#11498=CARTESIAN_POINT('Ctrl Pts',(-17.0582577813421,-3.72602328845455,
-1.39999999999999));
#11499=CARTESIAN_POINT('Ctrl Pts',(-16.8943723095674,-3.7266491009471,7.));
#11500=CARTESIAN_POINT('Ctrl Pts',(-16.8943723095674,-3.7266491009471,-1.39999999999999));
#11501=CARTESIAN_POINT('Ctrl Pts',(-16.7524120409277,-3.72194155665402,
7.));
#11502=CARTESIAN_POINT('Ctrl Pts',(-16.7524120409277,-3.72194155665402,
-1.39999999999999));
#11503=CARTESIAN_POINT('Ctrl Pts',(-16.632533556064,-3.7134461116587,7.));
#11504=CARTESIAN_POINT('Ctrl Pts',(-16.632533556064,-3.7134461116587,-1.39999999999999));
#11505=CARTESIAN_POINT('Ctrl Pts',(-16.5444222357228,-3.70408422142789,
7.));
#11506=CARTESIAN_POINT('Ctrl Pts',(-16.5444222357228,-3.70408422142789,
-1.39999999999999));
#11507=CARTESIAN_POINT('Ctrl Pts',(-16.4843881842109,-3.69552774561754,
7.));
#11508=CARTESIAN_POINT('Ctrl Pts',(-16.4843881842109,-3.69552774561754,
-1.39999999999999));
#11509=CARTESIAN_POINT('Ctrl Pts',(-16.4450105654964,-3.69014050504824,
7.));
#11510=CARTESIAN_POINT('Ctrl Pts',(-16.4450105654964,-3.69014050504824,
-1.39999999999999));
#11511=CARTESIAN_POINT('Ctrl Pts',(-16.409563995311,-3.68636158229544,7.));
#11512=CARTESIAN_POINT('Ctrl Pts',(-16.409563995311,-3.68636158229544,-1.39999999999999));
#11513=CARTESIAN_POINT('Ctrl Pts',(-16.3522749650865,-3.68169968173258,
7.));
#11514=CARTESIAN_POINT('Ctrl Pts',(-16.3522749650865,-3.68169968173258,
-1.39999999999999));
#11515=CARTESIAN_POINT('Ctrl Pts',(-16.2732984400115,-3.67963072201294,
7.));
#11516=CARTESIAN_POINT('Ctrl Pts',(-16.2732984400115,-3.67963072201294,
-1.39999999999999));
#11517=CARTESIAN_POINT('Ctrl Pts',(-16.1718717115691,-3.68733631276639,
7.));
#11518=CARTESIAN_POINT('Ctrl Pts',(-16.1718717115691,-3.68733631276639,
-1.39999999999999));
#11519=CARTESIAN_POINT('Ctrl Pts',(-16.0682204478862,-3.70904952755068,
7.));
#11520=CARTESIAN_POINT('Ctrl Pts',(-16.0682204478862,-3.70904952755068,
-1.39999999999999));
#11521=CARTESIAN_POINT('Ctrl Pts',(-15.958574817721,-3.75315043649995,7.));
#11522=CARTESIAN_POINT('Ctrl Pts',(-15.958574817721,-3.75315043649995,-1.39999999999999));
#11523=CARTESIAN_POINT('Ctrl Pts',(-15.8322454089585,-3.84407131175635,
7.));
#11524=CARTESIAN_POINT('Ctrl Pts',(-15.8322454089585,-3.84407131175635,
-1.39999999999999));
#11525=CARTESIAN_POINT('Ctrl Pts',(-15.7691023294921,-3.94611544431017,
7.));
#11526=CARTESIAN_POINT('Ctrl Pts',(-15.7691023294921,-3.94611544431017,
-1.39999999999999));
#11527=CARTESIAN_POINT('Ctrl Pts',(-15.7467591314705,-4.0127393206452,7.));
#11528=CARTESIAN_POINT('Ctrl Pts',(-15.7467591314705,-4.0127393206452,-1.39999999999999));
#11529=CARTESIAN_POINT('',(-15.7467591314705,-4.0127393206452,7.));
#11530=CARTESIAN_POINT('Origin',(0.,0.,7.));
#11531=CARTESIAN_POINT('',(-15.0980247376579,-6.00933848448149,7.));
#11532=CARTESIAN_POINT('Ctrl Pts',(-15.0980247376578,-6.00933848448161,
7.));
#11533=CARTESIAN_POINT('Ctrl Pts',(-15.0980247376578,-6.00933848448161,
-1.40000000000002));
#11534=CARTESIAN_POINT('Ctrl Pts',(-15.0769402326058,-6.07637133495397,
7.));
#11535=CARTESIAN_POINT('Ctrl Pts',(-15.0769402326058,-6.07637133495397,
-1.40000000000002));
#11536=CARTESIAN_POINT('Ctrl Pts',(-15.0680440207731,-6.19604134326091,
7.));
#11537=CARTESIAN_POINT('Ctrl Pts',(-15.0680440207731,-6.19604134326091,
-1.40000000000002));
#11538=CARTESIAN_POINT('Ctrl Pts',(-15.1168047097502,-6.34385243988823,
7.));
#11539=CARTESIAN_POINT('Ctrl Pts',(-15.1168047097502,-6.34385243988823,
-1.40000000000002));
#11540=CARTESIAN_POINT('Ctrl Pts',(-15.1795880240196,-6.44397890908498,
7.));
#11541=CARTESIAN_POINT('Ctrl Pts',(-15.1795880240196,-6.44397890908498,
-1.40000000000002));
#11542=CARTESIAN_POINT('Ctrl Pts',(-15.2506809503975,-6.52246995302231,
7.));
#11543=CARTESIAN_POINT('Ctrl Pts',(-15.2506809503975,-6.52246995302231,
-1.40000000000002));
#11544=CARTESIAN_POINT('Ctrl Pts',(-15.3282076647862,-6.58832104206025,
7.));
#11545=CARTESIAN_POINT('Ctrl Pts',(-15.3282076647862,-6.58832104206025,
-1.40000000000002));
#11546=CARTESIAN_POINT('Ctrl Pts',(-15.3933171197393,-6.63306845520279,
7.));
#11547=CARTESIAN_POINT('Ctrl Pts',(-15.3933171197393,-6.63306845520279,
-1.40000000000002));
#11548=CARTESIAN_POINT('Ctrl Pts',(-15.4424051151807,-6.66297054550545,
7.));
#11549=CARTESIAN_POINT('Ctrl Pts',(-15.4424051151807,-6.66297054550545,
-1.40000000000002));
#11550=CARTESIAN_POINT('Ctrl Pts',(-15.4733031879166,-6.68074830397729,
7.));
#11551=CARTESIAN_POINT('Ctrl Pts',(-15.4733031879166,-6.68074830397729,
-1.40000000000002));
#11552=CARTESIAN_POINT('Ctrl Pts',(-15.5083268912119,-6.69953551835472,
7.));
#11553=CARTESIAN_POINT('Ctrl Pts',(-15.5083268912119,-6.69953551835472,
-1.40000000000002));
#11554=CARTESIAN_POINT('Ctrl Pts',(-15.5619248294191,-6.72790031412626,
7.));
#11555=CARTESIAN_POINT('Ctrl Pts',(-15.5619248294191,-6.72790031412626,
-1.40000000000002));
#11556=CARTESIAN_POINT('Ctrl Pts',(-15.6387111659832,-6.77211692048665,
7.));
#11557=CARTESIAN_POINT('Ctrl Pts',(-15.6387111659832,-6.77211692048665,
-1.40000000000002));
#11558=CARTESIAN_POINT('Ctrl Pts',(-15.7406883947778,-6.8357067665807,7.));
#11559=CARTESIAN_POINT('Ctrl Pts',(-15.7406883947778,-6.8357067665807,-1.40000000000002));
#11560=CARTESIAN_POINT('Ctrl Pts',(-15.8583036897433,-6.91534043556372,
7.));
#11561=CARTESIAN_POINT('Ctrl Pts',(-15.8583036897433,-6.91534043556372,
-1.40000000000002));
#11562=CARTESIAN_POINT('Ctrl Pts',(-15.9905219781863,-7.01217619187965,
7.));
#11563=CARTESIAN_POINT('Ctrl Pts',(-15.9905219781863,-7.01217619187965,
-1.40000000000002));
#11564=CARTESIAN_POINT('Ctrl Pts',(-16.1361838672874,-7.12742326811382,
7.));
#11565=CARTESIAN_POINT('Ctrl Pts',(-16.1361838672874,-7.12742326811382,
-1.40000000000002));
#11566=CARTESIAN_POINT('Ctrl Pts',(-16.2940809887434,-7.26219165995681,
7.));
#11567=CARTESIAN_POINT('Ctrl Pts',(-16.2940809887434,-7.26219165995681,
-1.40000000000002));
#11568=CARTESIAN_POINT('Ctrl Pts',(-16.4629349257385,-7.41753779118423,
7.));
#11569=CARTESIAN_POINT('Ctrl Pts',(-16.4629349257385,-7.41753779118423,
-1.40000000000002));
#11570=CARTESIAN_POINT('Ctrl Pts',(-16.6414085620714,-7.59444470905136,
7.));
#11571=CARTESIAN_POINT('Ctrl Pts',(-16.6414085620714,-7.59444470905136,
-1.40000000000002));
#11572=CARTESIAN_POINT('Ctrl Pts',(-16.8766905033058,-7.84571320523309,
7.));
#11573=CARTESIAN_POINT('Ctrl Pts',(-16.8766905033058,-7.84571320523309,
-1.40000000000002));
#11574=CARTESIAN_POINT('Ctrl Pts',(-17.0448123137865,-8.04476736935674,
7.));
#11575=CARTESIAN_POINT('Ctrl Pts',(-17.0448123137865,-8.04476736935674,
-1.40000000000002));
#11576=CARTESIAN_POINT('Ctrl Pts',(-17.1502563092004,-8.1773289360728,7.));
#11577=CARTESIAN_POINT('Ctrl Pts',(-17.1502563092004,-8.1773289360728,-1.40000000000002));
#11578=CARTESIAN_POINT('',(-17.1502563092004,-8.1773289360728,7.));
#11579=CARTESIAN_POINT('Origin',(0.,0.,7.));
#11580=CARTESIAN_POINT('',(-16.6962658094609,-9.06833546026103,7.));
#11581=CARTESIAN_POINT('Ctrl Pts',(-16.6962658094608,-9.06833546026117,
7.));
#11582=CARTESIAN_POINT('Ctrl Pts',(-16.6962658094608,-9.06833546026117,
-1.39999999999999));
#11583=CARTESIAN_POINT('Ctrl Pts',(-16.5270428237395,-9.06094720995301,
7.));
#11584=CARTESIAN_POINT('Ctrl Pts',(-16.5270428237395,-9.06094720995301,
-1.39999999999999));
#11585=CARTESIAN_POINT('Ctrl Pts',(-16.2671851013731,-9.0419349102283,7.));
#11586=CARTESIAN_POINT('Ctrl Pts',(-16.2671851013731,-9.0419349102283,-1.39999999999999));
#11587=CARTESIAN_POINT('Ctrl Pts',(-15.9256093626227,-8.99927973772149,
7.));
#11588=CARTESIAN_POINT('Ctrl Pts',(-15.9256093626227,-8.99927973772149,
-1.39999999999999));
#11589=CARTESIAN_POINT('Ctrl Pts',(-15.6775844882862,-8.95887481023114,
7.));
#11590=CARTESIAN_POINT('Ctrl Pts',(-15.6775844882862,-8.95887481023114,
-1.39999999999999));
#11591=CARTESIAN_POINT('Ctrl Pts',(-15.4526569741556,-8.91357927057118,
7.));
#11592=CARTESIAN_POINT('Ctrl Pts',(-15.4526569741556,-8.91357927057118,
-1.39999999999999));
#11593=CARTESIAN_POINT('Ctrl Pts',(-15.2508174554788,-8.8650526891508,7.));
#11594=CARTESIAN_POINT('Ctrl Pts',(-15.2508174554788,-8.8650526891508,-1.39999999999999));
#11595=CARTESIAN_POINT('Ctrl Pts',(-15.0719627020186,-8.81495027721558,
7.));
#11596=CARTESIAN_POINT('Ctrl Pts',(-15.0719627020186,-8.81495027721558,
-1.39999999999999));
#11597=CARTESIAN_POINT('Ctrl Pts',(-14.9159049694657,-8.76490206435507,
7.));
#11598=CARTESIAN_POINT('Ctrl Pts',(-14.9159049694657,-8.76490206435507,
-1.39999999999999));
#11599=CARTESIAN_POINT('Ctrl Pts',(-14.7823474421093,-8.71655678814369,
7.));
#11600=CARTESIAN_POINT('Ctrl Pts',(-14.7823474421093,-8.71655678814369,
-1.39999999999999));
#11601=CARTESIAN_POINT('Ctrl Pts',(-14.6709614647944,-8.67143265073926,
7.));
#11602=CARTESIAN_POINT('Ctrl Pts',(-14.6709614647944,-8.67143265073926,
-1.39999999999999));
#11603=CARTESIAN_POINT('Ctrl Pts',(-14.5900556026053,-8.63530106864816,
7.));
#11604=CARTESIAN_POINT('Ctrl Pts',(-14.5900556026053,-8.63530106864816,
-1.39999999999999));
#11605=CARTESIAN_POINT('Ctrl Pts',(-14.5356039231527,-8.60861183441385,
7.));
#11606=CARTESIAN_POINT('Ctrl Pts',(-14.5356039231527,-8.60861183441385,
-1.39999999999999));
#11607=CARTESIAN_POINT('Ctrl Pts',(-14.4998183311667,-8.59131991078476,
7.));
#11608=CARTESIAN_POINT('Ctrl Pts',(-14.4998183311667,-8.59131991078476,
-1.39999999999999));
#11609=CARTESIAN_POINT('Ctrl Pts',(-14.4672743909627,-8.57677234909656,
7.));
#11610=CARTESIAN_POINT('Ctrl Pts',(-14.4672743909627,-8.57677234909656,
-1.39999999999999));
#11611=CARTESIAN_POINT('Ctrl Pts',(-14.4142298919554,-8.5546353342573,7.));
#11612=CARTESIAN_POINT('Ctrl Pts',(-14.4142298919554,-8.5546353342573,-1.39999999999999));
#11613=CARTESIAN_POINT('Ctrl Pts',(-14.3397580968625,-8.52826254822913,
7.));
#11614=CARTESIAN_POINT('Ctrl Pts',(-14.3397580968625,-8.52826254822913,
-1.39999999999999));
#11615=CARTESIAN_POINT('Ctrl Pts',(-14.2409143873564,-8.50424841775454,
7.));
#11616=CARTESIAN_POINT('Ctrl Pts',(-14.2409143873564,-8.50424841775454,
-1.39999999999999));
#11617=CARTESIAN_POINT('Ctrl Pts',(-14.1356264252376,-8.4928689101984,7.));
#11618=CARTESIAN_POINT('Ctrl Pts',(-14.1356264252376,-8.4928689101984,-1.39999999999999));
#11619=CARTESIAN_POINT('Ctrl Pts',(-14.0177193038531,-8.50092900394916,
7.));
#11620=CARTESIAN_POINT('Ctrl Pts',(-14.0177193038531,-8.50092900394916,
-1.39999999999999));
#11621=CARTESIAN_POINT('Ctrl Pts',(-13.8694768008521,-8.54836196063206,
7.));
#11622=CARTESIAN_POINT('Ctrl Pts',(-13.8694768008521,-8.54836196063206,
-1.39999999999999));
#11623=CARTESIAN_POINT('Ctrl Pts',(-13.7778907925313,-8.62589941321478,
7.));
#11624=CARTESIAN_POINT('Ctrl Pts',(-13.7778907925313,-8.62589941321478,
-1.39999999999999));
#11625=CARTESIAN_POINT('Ctrl Pts',(-13.7360532384392,-8.68235805704666,
7.));
#11626=CARTESIAN_POINT('Ctrl Pts',(-13.7360532384392,-8.68235805704666,
-1.39999999999999));
#11627=CARTESIAN_POINT('',(-13.7360532384392,-8.68235805704666,7.));
#11628=CARTESIAN_POINT('Origin',(0.,0.,7.));
#11629=CARTESIAN_POINT('',(-12.5020870932788,-10.380766749719,7.));
#11630=CARTESIAN_POINT('Ctrl Pts',(-12.5020870932787,-10.3807667497191,
7.));
#11631=CARTESIAN_POINT('Ctrl Pts',(-12.5020870932787,-10.3807667497191,
-1.4));
#11632=CARTESIAN_POINT('Ctrl Pts',(-12.4613202473788,-10.4380033085876,
7.));
#11633=CARTESIAN_POINT('Ctrl Pts',(-12.4613202473788,-10.4380033085876,
-1.4));
#11634=CARTESIAN_POINT('Ctrl Pts',(-12.4158793808611,-10.5490671691512,
7.));
#11635=CARTESIAN_POINT('Ctrl Pts',(-12.4158793808611,-10.5490671691512,
-1.4));
#11636=CARTESIAN_POINT('Ctrl Pts',(-12.4165774110367,-10.7047117573306,
7.));
#11637=CARTESIAN_POINT('Ctrl Pts',(-12.4165774110367,-10.7047117573306,
-1.4));
#11638=CARTESIAN_POINT('Ctrl Pts',(-12.4453471106188,-10.8193387993863,
7.));
#11639=CARTESIAN_POINT('Ctrl Pts',(-12.4453471106188,-10.8193387993863,
-1.4));
#11640=CARTESIAN_POINT('Ctrl Pts',(-12.4887054350301,-10.9159571406243,
7.));
#11641=CARTESIAN_POINT('Ctrl Pts',(-12.4887054350301,-10.9159571406243,
-1.4));
#11642=CARTESIAN_POINT('Ctrl Pts',(-12.5420886163255,-11.0025423202231,
7.));
#11643=CARTESIAN_POINT('Ctrl Pts',(-12.5420886163255,-11.0025423202231,
-1.4));
#11644=CARTESIAN_POINT('Ctrl Pts',(-12.5901836766158,-11.0652195671547,
7.));
#11645=CARTESIAN_POINT('Ctrl Pts',(-12.5901836766158,-11.0652195671547,
-1.4));
#11646=CARTESIAN_POINT('Ctrl Pts',(-12.6276288804813,-11.1088271697991,
7.));
#11647=CARTESIAN_POINT('Ctrl Pts',(-12.6276288804813,-11.1088271697991,
-1.4));
#11648=CARTESIAN_POINT('Ctrl Pts',(-12.6515210644081,-11.1352828524077,
7.));
#11649=CARTESIAN_POINT('Ctrl Pts',(-12.6515210644081,-11.1352828524077,
-1.4));
#11650=CARTESIAN_POINT('Ctrl Pts',(-12.6790250171322,-11.1639734745885,
7.));
#11651=CARTESIAN_POINT('Ctrl Pts',(-12.6790250171322,-11.1639734745885,
-1.4));
#11652=CARTESIAN_POINT('Ctrl Pts',(-12.7212344815888,-11.2075126722099,
7.));
#11653=CARTESIAN_POINT('Ctrl Pts',(-12.7212344815888,-11.2075126722099,
-1.4));
#11654=CARTESIAN_POINT('Ctrl Pts',(-12.7805989445416,-11.2732934467515,
7.));
#11655=CARTESIAN_POINT('Ctrl Pts',(-12.7805989445416,-11.2732934467515,
-1.4));
#11656=CARTESIAN_POINT('Ctrl Pts',(-12.8579347093876,-11.3652836809863,
7.));
#11657=CARTESIAN_POINT('Ctrl Pts',(-12.8579347093876,-11.3652836809863,
-1.4));
#11658=CARTESIAN_POINT('Ctrl Pts',(-12.9451853450404,-11.4773649257318,
7.));
#11659=CARTESIAN_POINT('Ctrl Pts',(-12.9451853450404,-11.4773649257318,
-1.4));
#11660=CARTESIAN_POINT('Ctrl Pts',(-13.0410085154727,-11.6103189008825,
7.));
#11661=CARTESIAN_POINT('Ctrl Pts',(-13.0410085154727,-11.6103189008825,
-1.4));
#11662=CARTESIAN_POINT('Ctrl Pts',(-13.1439278991698,-11.764937382884,7.));
#11663=CARTESIAN_POINT('Ctrl Pts',(-13.1439278991698,-11.764937382884,-1.4));
#11664=CARTESIAN_POINT('Ctrl Pts',(-13.2524512620508,-11.9419026340297,
7.));
#11665=CARTESIAN_POINT('Ctrl Pts',(-13.2524512620508,-11.9419026340297,
-1.4));
#11666=CARTESIAN_POINT('Ctrl Pts',(-13.3650363045724,-12.1418243205134,
7.));
#11667=CARTESIAN_POINT('Ctrl Pts',(-13.3650363045724,-12.1418243205134,
-1.4));
#11668=CARTESIAN_POINT('Ctrl Pts',(-13.4801075753502,-12.3652241842034,
7.));
#11669=CARTESIAN_POINT('Ctrl Pts',(-13.4801075753502,-12.3652241842034,
-1.4));
#11670=CARTESIAN_POINT('Ctrl Pts',(-13.6262277632565,-12.6769008431476,
7.));
#11671=CARTESIAN_POINT('Ctrl Pts',(-13.6262277632565,-12.6769008431476,
-1.4));
#11672=CARTESIAN_POINT('Ctrl Pts',(-13.7246099871303,-12.9181650995967,
7.));
#11673=CARTESIAN_POINT('Ctrl Pts',(-13.7246099871303,-12.9181650995967,
-1.4));
#11674=CARTESIAN_POINT('Ctrl Pts',(-13.7839294091566,-13.07682262797,7.));
#11675=CARTESIAN_POINT('Ctrl Pts',(-13.7839294091566,-13.07682262797,-1.4));
#11676=CARTESIAN_POINT('',(-13.7839294091566,-13.07682262797,7.));
#11677=CARTESIAN_POINT('Origin',(0.,0.,7.));
#11678=CARTESIAN_POINT('',(-13.0768226279701,-13.7839294091565,7.));
#11679=CARTESIAN_POINT('Ctrl Pts',(-13.07682262797,-13.7839294091566,7.));
#11680=CARTESIAN_POINT('Ctrl Pts',(-13.07682262797,-13.7839294091566,-1.39999999999999));
#11681=CARTESIAN_POINT('Ctrl Pts',(-12.9181650995967,-13.7246099871302,
7.));
#11682=CARTESIAN_POINT('Ctrl Pts',(-12.9181650995967,-13.7246099871302,
-1.39999999999999));
#11683=CARTESIAN_POINT('Ctrl Pts',(-12.6769008431476,-13.6262277632565,
7.));
#11684=CARTESIAN_POINT('Ctrl Pts',(-12.6769008431476,-13.6262277632565,
-1.39999999999999));
#11685=CARTESIAN_POINT('Ctrl Pts',(-12.3652241842034,-13.4801075753502,
7.));
#11686=CARTESIAN_POINT('Ctrl Pts',(-12.3652241842034,-13.4801075753502,
-1.39999999999999));
#11687=CARTESIAN_POINT('Ctrl Pts',(-12.1418243205134,-13.3650363045723,
7.));
#11688=CARTESIAN_POINT('Ctrl Pts',(-12.1418243205134,-13.3650363045723,
-1.39999999999999));
#11689=CARTESIAN_POINT('Ctrl Pts',(-11.9419026340297,-13.2524512620508,
7.));
#11690=CARTESIAN_POINT('Ctrl Pts',(-11.9419026340297,-13.2524512620508,
-1.39999999999999));
#11691=CARTESIAN_POINT('Ctrl Pts',(-11.764937382884,-13.1439278991698,7.));
#11692=CARTESIAN_POINT('Ctrl Pts',(-11.764937382884,-13.1439278991698,-1.39999999999999));
#11693=CARTESIAN_POINT('Ctrl Pts',(-11.6103189008825,-13.0410085154728,
7.));
#11694=CARTESIAN_POINT('Ctrl Pts',(-11.6103189008825,-13.0410085154728,
-1.39999999999999));
#11695=CARTESIAN_POINT('Ctrl Pts',(-11.4773649257318,-12.9451853450404,
7.));
#11696=CARTESIAN_POINT('Ctrl Pts',(-11.4773649257318,-12.9451853450404,
-1.39999999999999));
#11697=CARTESIAN_POINT('Ctrl Pts',(-11.3652836809863,-12.8579347093876,
7.));
#11698=CARTESIAN_POINT('Ctrl Pts',(-11.3652836809863,-12.8579347093876,
-1.39999999999999));
#11699=CARTESIAN_POINT('Ctrl Pts',(-11.2732934467515,-12.7805989445416,
7.));
#11700=CARTESIAN_POINT('Ctrl Pts',(-11.2732934467515,-12.7805989445416,
-1.39999999999999));
#11701=CARTESIAN_POINT('Ctrl Pts',(-11.2075126722099,-12.7212344815888,
7.));
#11702=CARTESIAN_POINT('Ctrl Pts',(-11.2075126722099,-12.7212344815888,
-1.39999999999999));
#11703=CARTESIAN_POINT('Ctrl Pts',(-11.1639734745886,-12.6790250171322,
7.));
#11704=CARTESIAN_POINT('Ctrl Pts',(-11.1639734745886,-12.6790250171322,
-1.39999999999999));
#11705=CARTESIAN_POINT('Ctrl Pts',(-11.1352828524077,-12.651521064408,7.));
#11706=CARTESIAN_POINT('Ctrl Pts',(-11.1352828524077,-12.651521064408,-1.39999999999999));
#11707=CARTESIAN_POINT('Ctrl Pts',(-11.1088271697991,-12.6276288804813,
7.));
#11708=CARTESIAN_POINT('Ctrl Pts',(-11.1088271697991,-12.6276288804813,
-1.39999999999999));
#11709=CARTESIAN_POINT('Ctrl Pts',(-11.0652195671547,-12.5901836766158,
7.));
#11710=CARTESIAN_POINT('Ctrl Pts',(-11.0652195671547,-12.5901836766158,
-1.39999999999999));
#11711=CARTESIAN_POINT('Ctrl Pts',(-11.0025423202231,-12.5420886163255,
7.));
#11712=CARTESIAN_POINT('Ctrl Pts',(-11.0025423202231,-12.5420886163255,
-1.39999999999999));
#11713=CARTESIAN_POINT('Ctrl Pts',(-10.9159571406243,-12.48870543503,7.));
#11714=CARTESIAN_POINT('Ctrl Pts',(-10.9159571406243,-12.48870543503,-1.39999999999999));
#11715=CARTESIAN_POINT('Ctrl Pts',(-10.8193387993863,-12.4453471106187,
7.));
#11716=CARTESIAN_POINT('Ctrl Pts',(-10.8193387993863,-12.4453471106187,
-1.39999999999999));
#11717=CARTESIAN_POINT('Ctrl Pts',(-10.7047117573307,-12.4165774110367,
7.));
#11718=CARTESIAN_POINT('Ctrl Pts',(-10.7047117573307,-12.4165774110367,
-1.39999999999999));
#11719=CARTESIAN_POINT('Ctrl Pts',(-10.5490671691512,-12.4158793808611,
7.));
#11720=CARTESIAN_POINT('Ctrl Pts',(-10.5490671691512,-12.4158793808611,
-1.39999999999999));
#11721=CARTESIAN_POINT('Ctrl Pts',(-10.4380033085876,-12.4613202473787,
7.));
#11722=CARTESIAN_POINT('Ctrl Pts',(-10.4380033085876,-12.4613202473787,
-1.39999999999999));
#11723=CARTESIAN_POINT('Ctrl Pts',(-10.3807667497191,-12.5020870932787,
7.));
#11724=CARTESIAN_POINT('Ctrl Pts',(-10.3807667497191,-12.5020870932787,
-1.39999999999999));
#11725=CARTESIAN_POINT('',(-10.3807667497191,-12.5020870932787,7.));
#11726=CARTESIAN_POINT('Origin',(0.,0.,7.));
#11727=CARTESIAN_POINT('',(-8.68235805704677,-13.7360532384392,7.));
#11728=CARTESIAN_POINT('Ctrl Pts',(-8.68235805704668,-13.7360532384392,
7.));
#11729=CARTESIAN_POINT('Ctrl Pts',(-8.68235805704668,-13.7360532384392,
-1.39999999999998));
#11730=CARTESIAN_POINT('Ctrl Pts',(-8.62589941321481,-13.7778907925313,
7.));
#11731=CARTESIAN_POINT('Ctrl Pts',(-8.62589941321481,-13.7778907925313,
-1.39999999999998));
#11732=CARTESIAN_POINT('Ctrl Pts',(-8.54836196063208,-13.8694768008521,
7.));
#11733=CARTESIAN_POINT('Ctrl Pts',(-8.54836196063208,-13.8694768008521,
-1.39999999999998));
#11734=CARTESIAN_POINT('Ctrl Pts',(-8.50092900394921,-14.0177193038531,
7.));
#11735=CARTESIAN_POINT('Ctrl Pts',(-8.50092900394921,-14.0177193038531,
-1.39999999999998));
#11736=CARTESIAN_POINT('Ctrl Pts',(-8.49286891019844,-14.1356264252377,
7.));
#11737=CARTESIAN_POINT('Ctrl Pts',(-8.49286891019844,-14.1356264252377,
-1.39999999999998));
#11738=CARTESIAN_POINT('Ctrl Pts',(-8.50424841775456,-14.2409143873564,
7.));
#11739=CARTESIAN_POINT('Ctrl Pts',(-8.50424841775456,-14.2409143873564,
-1.39999999999998));
#11740=CARTESIAN_POINT('Ctrl Pts',(-8.52826254822915,-14.3397580968626,
7.));
#11741=CARTESIAN_POINT('Ctrl Pts',(-8.52826254822915,-14.3397580968626,
-1.39999999999998));
#11742=CARTESIAN_POINT('Ctrl Pts',(-8.55463533425732,-14.4142298919555,
7.));
#11743=CARTESIAN_POINT('Ctrl Pts',(-8.55463533425732,-14.4142298919555,
-1.39999999999998));
#11744=CARTESIAN_POINT('Ctrl Pts',(-8.57677234909656,-14.4672743909627,
7.));
#11745=CARTESIAN_POINT('Ctrl Pts',(-8.57677234909656,-14.4672743909627,
-1.39999999999998));
#11746=CARTESIAN_POINT('Ctrl Pts',(-8.59131991078476,-14.4998183311667,
7.));
#11747=CARTESIAN_POINT('Ctrl Pts',(-8.59131991078476,-14.4998183311667,
-1.39999999999998));
#11748=CARTESIAN_POINT('Ctrl Pts',(-8.6086118344139,-14.5356039231527,7.));
#11749=CARTESIAN_POINT('Ctrl Pts',(-8.6086118344139,-14.5356039231527,-1.39999999999998));
#11750=CARTESIAN_POINT('Ctrl Pts',(-8.63530106864818,-14.5900556026053,
7.));
#11751=CARTESIAN_POINT('Ctrl Pts',(-8.63530106864818,-14.5900556026053,
-1.39999999999998));
#11752=CARTESIAN_POINT('Ctrl Pts',(-8.67143265073928,-14.6709614647944,
7.));
#11753=CARTESIAN_POINT('Ctrl Pts',(-8.67143265073928,-14.6709614647944,
-1.39999999999998));
#11754=CARTESIAN_POINT('Ctrl Pts',(-8.71655678814373,-14.7823474421093,
7.));
#11755=CARTESIAN_POINT('Ctrl Pts',(-8.71655678814373,-14.7823474421093,
-1.39999999999998));
#11756=CARTESIAN_POINT('Ctrl Pts',(-8.76490206435509,-14.9159049694657,
7.));
#11757=CARTESIAN_POINT('Ctrl Pts',(-8.76490206435509,-14.9159049694657,
-1.39999999999998));
#11758=CARTESIAN_POINT('Ctrl Pts',(-8.81495027721557,-15.0719627020186,
7.));
#11759=CARTESIAN_POINT('Ctrl Pts',(-8.81495027721557,-15.0719627020186,
-1.39999999999998));
#11760=CARTESIAN_POINT('Ctrl Pts',(-8.86505268915084,-15.2508174554788,
7.));
#11761=CARTESIAN_POINT('Ctrl Pts',(-8.86505268915084,-15.2508174554788,
-1.39999999999998));
#11762=CARTESIAN_POINT('Ctrl Pts',(-8.91357927057117,-15.4526569741556,
7.));
#11763=CARTESIAN_POINT('Ctrl Pts',(-8.91357927057117,-15.4526569741556,
-1.39999999999998));
#11764=CARTESIAN_POINT('Ctrl Pts',(-8.95887481023116,-15.6775844882862,
7.));
#11765=CARTESIAN_POINT('Ctrl Pts',(-8.95887481023116,-15.6775844882862,
-1.39999999999998));
#11766=CARTESIAN_POINT('Ctrl Pts',(-8.99927973772154,-15.9256093626227,
7.));
#11767=CARTESIAN_POINT('Ctrl Pts',(-8.99927973772154,-15.9256093626227,
-1.39999999999998));
#11768=CARTESIAN_POINT('Ctrl Pts',(-9.04193491022832,-16.2671851013731,
7.));
#11769=CARTESIAN_POINT('Ctrl Pts',(-9.04193491022832,-16.2671851013731,
-1.39999999999998));
#11770=CARTESIAN_POINT('Ctrl Pts',(-9.06094720995306,-16.5270428237395,
7.));
#11771=CARTESIAN_POINT('Ctrl Pts',(-9.06094720995306,-16.5270428237395,
-1.39999999999998));
#11772=CARTESIAN_POINT('Ctrl Pts',(-9.06833546026116,-16.6962658094608,
7.));
#11773=CARTESIAN_POINT('Ctrl Pts',(-9.06833546026116,-16.6962658094608,
-1.39999999999998));
#11774=CARTESIAN_POINT('',(-9.06833546026116,-16.6962658094608,7.));
#11775=CARTESIAN_POINT('Origin',(0.,0.,7.));
#11776=CARTESIAN_POINT('',(-8.17732893607292,-17.1502563092003,7.));
#11777=CARTESIAN_POINT('Ctrl Pts',(-8.1773289360728,-17.1502563092004,7.));
#11778=CARTESIAN_POINT('Ctrl Pts',(-8.1773289360728,-17.1502563092004,-1.39999999999998));
#11779=CARTESIAN_POINT('Ctrl Pts',(-8.04476736935674,-17.0448123137865,
7.));
#11780=CARTESIAN_POINT('Ctrl Pts',(-8.04476736935674,-17.0448123137865,
-1.39999999999998));
#11781=CARTESIAN_POINT('Ctrl Pts',(-7.8457132052331,-16.8766905033057,7.));
#11782=CARTESIAN_POINT('Ctrl Pts',(-7.8457132052331,-16.8766905033057,-1.39999999999998));
#11783=CARTESIAN_POINT('Ctrl Pts',(-7.59444470905137,-16.6414085620714,
7.));
#11784=CARTESIAN_POINT('Ctrl Pts',(-7.59444470905137,-16.6414085620714,
-1.39999999999998));
#11785=CARTESIAN_POINT('Ctrl Pts',(-7.41753779118422,-16.4629349257385,
7.));
#11786=CARTESIAN_POINT('Ctrl Pts',(-7.41753779118422,-16.4629349257385,
-1.39999999999998));
#11787=CARTESIAN_POINT('Ctrl Pts',(-7.2621916599568,-16.2940809887434,7.));
#11788=CARTESIAN_POINT('Ctrl Pts',(-7.2621916599568,-16.2940809887434,-1.39999999999998));
#11789=CARTESIAN_POINT('Ctrl Pts',(-7.12742326811384,-16.1361838672874,
7.));
#11790=CARTESIAN_POINT('Ctrl Pts',(-7.12742326811384,-16.1361838672874,
-1.39999999999998));
#11791=CARTESIAN_POINT('Ctrl Pts',(-7.01217619187963,-15.9905219781863,
7.));
#11792=CARTESIAN_POINT('Ctrl Pts',(-7.01217619187963,-15.9905219781863,
-1.39999999999998));
#11793=CARTESIAN_POINT('Ctrl Pts',(-6.9153404355637,-15.8583036897432,7.));
#11794=CARTESIAN_POINT('Ctrl Pts',(-6.9153404355637,-15.8583036897432,-1.39999999999998));
#11795=CARTESIAN_POINT('Ctrl Pts',(-6.8357067665807,-15.7406883947777,7.));
#11796=CARTESIAN_POINT('Ctrl Pts',(-6.8357067665807,-15.7406883947777,-1.39999999999998));
#11797=CARTESIAN_POINT('Ctrl Pts',(-6.77211692048664,-15.6387111659832,
7.));
#11798=CARTESIAN_POINT('Ctrl Pts',(-6.77211692048664,-15.6387111659832,
-1.39999999999998));
#11799=CARTESIAN_POINT('Ctrl Pts',(-6.72790031412625,-15.5619248294191,
7.));
#11800=CARTESIAN_POINT('Ctrl Pts',(-6.72790031412625,-15.5619248294191,
-1.39999999999998));
#11801=CARTESIAN_POINT('Ctrl Pts',(-6.69953551835473,-15.5083268912118,
7.));
#11802=CARTESIAN_POINT('Ctrl Pts',(-6.69953551835473,-15.5083268912118,
-1.39999999999998));
#11803=CARTESIAN_POINT('Ctrl Pts',(-6.68074830397727,-15.4733031879166,
7.));
#11804=CARTESIAN_POINT('Ctrl Pts',(-6.68074830397727,-15.4733031879166,
-1.39999999999998));
#11805=CARTESIAN_POINT('Ctrl Pts',(-6.66297054550543,-15.4424051151807,
7.));
#11806=CARTESIAN_POINT('Ctrl Pts',(-6.66297054550543,-15.4424051151807,
-1.39999999999998));
#11807=CARTESIAN_POINT('Ctrl Pts',(-6.63306845520277,-15.3933171197393,
7.));
#11808=CARTESIAN_POINT('Ctrl Pts',(-6.63306845520277,-15.3933171197393,
-1.39999999999998));
#11809=CARTESIAN_POINT('Ctrl Pts',(-6.58832104206024,-15.3282076647861,
7.));
#11810=CARTESIAN_POINT('Ctrl Pts',(-6.58832104206024,-15.3282076647861,
-1.39999999999998));
#11811=CARTESIAN_POINT('Ctrl Pts',(-6.52246995302227,-15.2506809503975,
7.));
#11812=CARTESIAN_POINT('Ctrl Pts',(-6.52246995302227,-15.2506809503975,
-1.39999999999998));
#11813=CARTESIAN_POINT('Ctrl Pts',(-6.44397890908497,-15.1795880240196,
7.));
#11814=CARTESIAN_POINT('Ctrl Pts',(-6.44397890908497,-15.1795880240196,
-1.39999999999998));
#11815=CARTESIAN_POINT('Ctrl Pts',(-6.34385243988824,-15.1168047097501,
7.));
#11816=CARTESIAN_POINT('Ctrl Pts',(-6.34385243988824,-15.1168047097501,
-1.39999999999998));
#11817=CARTESIAN_POINT('Ctrl Pts',(-6.19604134326091,-15.0680440207731,
7.));
#11818=CARTESIAN_POINT('Ctrl Pts',(-6.19604134326091,-15.0680440207731,
-1.39999999999998));
#11819=CARTESIAN_POINT('Ctrl Pts',(-6.07637133495395,-15.0769402326058,
7.));
#11820=CARTESIAN_POINT('Ctrl Pts',(-6.07637133495395,-15.0769402326058,
-1.39999999999998));
#11821=CARTESIAN_POINT('Ctrl Pts',(-6.0093384844816,-15.0980247376578,7.));
#11822=CARTESIAN_POINT('Ctrl Pts',(-6.0093384844816,-15.0980247376578,-1.39999999999998));
#11823=CARTESIAN_POINT('',(-6.0093384844816,-15.0980247376578,7.));
#11824=CARTESIAN_POINT('Origin',(0.,0.,7.));
#11825=CARTESIAN_POINT('',(-4.01273932064531,-15.7467591314704,7.));
#11826=CARTESIAN_POINT('Ctrl Pts',(-4.01273932064524,-15.7467591314704,
7.));
#11827=CARTESIAN_POINT('Ctrl Pts',(-4.01273932064524,-15.7467591314704,
-1.39999999999997));
#11828=CARTESIAN_POINT('Ctrl Pts',(-3.94611544431022,-15.7691023294921,
7.));
#11829=CARTESIAN_POINT('Ctrl Pts',(-3.94611544431022,-15.7691023294921,
-1.39999999999997));
#11830=CARTESIAN_POINT('Ctrl Pts',(-3.8440713117564,-15.8322454089585,7.));
#11831=CARTESIAN_POINT('Ctrl Pts',(-3.8440713117564,-15.8322454089585,-1.39999999999997));
#11832=CARTESIAN_POINT('Ctrl Pts',(-3.75315043650002,-15.958574817721,7.));
#11833=CARTESIAN_POINT('Ctrl Pts',(-3.75315043650002,-15.958574817721,-1.39999999999997));
#11834=CARTESIAN_POINT('Ctrl Pts',(-3.70904952755073,-16.0682204478862,
7.));
#11835=CARTESIAN_POINT('Ctrl Pts',(-3.70904952755073,-16.0682204478862,
-1.39999999999997));
#11836=CARTESIAN_POINT('Ctrl Pts',(-3.68733631276642,-16.1718717115691,
7.));
#11837=CARTESIAN_POINT('Ctrl Pts',(-3.68733631276642,-16.1718717115691,
-1.39999999999997));
#11838=CARTESIAN_POINT('Ctrl Pts',(-3.67963072201298,-16.2732984400115,
7.));
#11839=CARTESIAN_POINT('Ctrl Pts',(-3.67963072201298,-16.2732984400115,
-1.39999999999997));
#11840=CARTESIAN_POINT('Ctrl Pts',(-3.68169968173261,-16.3522749650865,
7.));
#11841=CARTESIAN_POINT('Ctrl Pts',(-3.68169968173261,-16.3522749650865,
-1.39999999999997));
#11842=CARTESIAN_POINT('Ctrl Pts',(-3.68636158229546,-16.409563995311,7.));
#11843=CARTESIAN_POINT('Ctrl Pts',(-3.68636158229546,-16.409563995311,-1.39999999999997));
#11844=CARTESIAN_POINT('Ctrl Pts',(-3.69014050504826,-16.4450105654963,
7.));
#11845=CARTESIAN_POINT('Ctrl Pts',(-3.69014050504826,-16.4450105654963,
-1.39999999999997));
#11846=CARTESIAN_POINT('Ctrl Pts',(-3.6955277456176,-16.4843881842109,7.));
#11847=CARTESIAN_POINT('Ctrl Pts',(-3.6955277456176,-16.4843881842109,-1.39999999999997));
#11848=CARTESIAN_POINT('Ctrl Pts',(-3.70408422142792,-16.5444222357228,
7.));
#11849=CARTESIAN_POINT('Ctrl Pts',(-3.70408422142792,-16.5444222357228,
-1.39999999999997));
#11850=CARTESIAN_POINT('Ctrl Pts',(-3.71344611165872,-16.632533556064,7.));
#11851=CARTESIAN_POINT('Ctrl Pts',(-3.71344611165872,-16.632533556064,-1.39999999999997));
#11852=CARTESIAN_POINT('Ctrl Pts',(-3.72194155665407,-16.7524120409277,
7.));
#11853=CARTESIAN_POINT('Ctrl Pts',(-3.72194155665407,-16.7524120409277,
-1.39999999999997));
#11854=CARTESIAN_POINT('Ctrl Pts',(-3.72664910094713,-16.8943723095674,
7.));
#11855=CARTESIAN_POINT('Ctrl Pts',(-3.72664910094713,-16.8943723095674,
-1.39999999999997));
#11856=CARTESIAN_POINT('Ctrl Pts',(-3.72602328845455,-17.0582577813421,
7.));
#11857=CARTESIAN_POINT('Ctrl Pts',(-3.72602328845455,-17.0582577813421,
-1.39999999999997));
#11858=CARTESIAN_POINT('Ctrl Pts',(-3.71840435546375,-17.2438412568379,
7.));
#11859=CARTESIAN_POINT('Ctrl Pts',(-3.71840435546375,-17.2438412568379,
-1.39999999999997));
#11860=CARTESIAN_POINT('Ctrl Pts',(-3.70218403552949,-17.4507975846592,
7.));
#11861=CARTESIAN_POINT('Ctrl Pts',(-3.70218403552949,-17.4507975846592,
-1.39999999999997));
#11862=CARTESIAN_POINT('Ctrl Pts',(-3.67575622931335,-17.6787134541915,
7.));
#11863=CARTESIAN_POINT('Ctrl Pts',(-3.67575622931335,-17.6787134541915,
-1.39999999999997));
#11864=CARTESIAN_POINT('Ctrl Pts',(-3.63753969769582,-17.9270849363835,
7.));
#11865=CARTESIAN_POINT('Ctrl Pts',(-3.63753969769582,-17.9270849363835,
-1.39999999999997));
#11866=CARTESIAN_POINT('Ctrl Pts',(-3.57255446932205,-18.265123941733,7.));
#11867=CARTESIAN_POINT('Ctrl Pts',(-3.57255446932205,-18.265123941733,-1.39999999999997));
#11868=CARTESIAN_POINT('Ctrl Pts',(-3.51033578853422,-18.5181384456163,
7.));
#11869=CARTESIAN_POINT('Ctrl Pts',(-3.51033578853422,-18.5181384456163,
-1.39999999999997));
#11870=CARTESIAN_POINT('Ctrl Pts',(-3.46506965370701,-18.6813621637973,
7.));
#11871=CARTESIAN_POINT('Ctrl Pts',(-3.46506965370701,-18.6813621637973,
-1.39999999999997));
#11872=CARTESIAN_POINT('',(-3.46506965370701,-18.6813621637973,7.));
#11873=CARTESIAN_POINT('Origin',(0.,0.,7.));
#11874=CARTESIAN_POINT('',(-2.47738131311198,-18.8377966288376,7.));
#11875=CARTESIAN_POINT('Ctrl Pts',(-2.47738131311189,-18.8377966288376,
7.));
#11876=CARTESIAN_POINT('Ctrl Pts',(-2.47738131311189,-18.8377966288376,
-1.39999999999999));
#11877=CARTESIAN_POINT('Ctrl Pts',(-2.38389175781398,-18.6965496529788,
7.));
#11878=CARTESIAN_POINT('Ctrl Pts',(-2.38389175781398,-18.6965496529788,
-1.39999999999999));
#11879=CARTESIAN_POINT('Ctrl Pts',(-2.24653249449213,-18.4751451900744,
7.));
#11880=CARTESIAN_POINT('Ctrl Pts',(-2.24653249449213,-18.4751451900744,
-1.39999999999999));
#11881=CARTESIAN_POINT('Ctrl Pts',(-2.08026807216976,-18.1737325312257,
7.));
#11882=CARTESIAN_POINT('Ctrl Pts',(-2.08026807216976,-18.1737325312257,
-1.39999999999999));
#11883=CARTESIAN_POINT('Ctrl Pts',(-1.96717098182926,-17.949326772361,7.));
#11884=CARTESIAN_POINT('Ctrl Pts',(-1.96717098182926,-17.949326772361,-1.39999999999999));
#11885=CARTESIAN_POINT('Ctrl Pts',(-1.87160676754278,-17.7407325407201,
7.));
#11886=CARTESIAN_POINT('Ctrl Pts',(-1.87160676754278,-17.7407325407201,
-1.39999999999999));
#11887=CARTESIAN_POINT('Ctrl Pts',(-1.79222730418273,-17.548917731071,7.));
#11888=CARTESIAN_POINT('Ctrl Pts',(-1.79222730418273,-17.548917731071,-1.39999999999999));
#11889=CARTESIAN_POINT('Ctrl Pts',(-1.7276328205112,-17.3747717371572,7.));
#11890=CARTESIAN_POINT('Ctrl Pts',(-1.7276328205112,-17.3747717371572,-1.39999999999999));
#11891=CARTESIAN_POINT('Ctrl Pts',(-1.67639424155264,-17.2191007779952,
7.));
#11892=CARTESIAN_POINT('Ctrl Pts',(-1.67639424155264,-17.2191007779952,
-1.39999999999999));
#11893=CARTESIAN_POINT('Ctrl Pts',(-1.63700324669264,-17.0826338282621,
7.));
#11894=CARTESIAN_POINT('Ctrl Pts',(-1.63700324669264,-17.0826338282621,
-1.39999999999999));
#11895=CARTESIAN_POINT('Ctrl Pts',(-1.60803840593146,-16.9659973771906,
7.));
#11896=CARTESIAN_POINT('Ctrl Pts',(-1.60803840593146,-16.9659973771906,
-1.39999999999999));
#11897=CARTESIAN_POINT('Ctrl Pts',(-1.58971419725806,-16.8793055486399,
7.));
#11898=CARTESIAN_POINT('Ctrl Pts',(-1.58971419725806,-16.8793055486399,
-1.39999999999999));
#11899=CARTESIAN_POINT('Ctrl Pts',(-1.57930034717566,-16.8195656763126,
7.));
#11900=CARTESIAN_POINT('Ctrl Pts',(-1.57930034717566,-16.8195656763126,
-1.39999999999999));
#11901=CARTESIAN_POINT('Ctrl Pts',(-1.57225556404312,-16.7804505865492,
7.));
#11902=CARTESIAN_POINT('Ctrl Pts',(-1.57225556404312,-16.7804505865492,
-1.39999999999999));
#11903=CARTESIAN_POINT('Ctrl Pts',(-1.56489594057218,-16.7455711436431,
7.));
#11904=CARTESIAN_POINT('Ctrl Pts',(-1.56489594057218,-16.7455711436431,
-1.39999999999999));
#11905=CARTESIAN_POINT('Ctrl Pts',(-1.55162638755018,-16.6896454316358,
7.));
#11906=CARTESIAN_POINT('Ctrl Pts',(-1.55162638755018,-16.6896454316358,
-1.39999999999999));
#11907=CARTESIAN_POINT('Ctrl Pts',(-1.52918899676863,-16.6138949491149,
7.));
#11908=CARTESIAN_POINT('Ctrl Pts',(-1.52918899676863,-16.6138949491149,
-1.39999999999999));
#11909=CARTESIAN_POINT('Ctrl Pts',(-1.49051796169811,-16.5198135565977,
7.));
#11910=CARTESIAN_POINT('Ctrl Pts',(-1.49051796169811,-16.5198135565977,
-1.39999999999999));
#11911=CARTESIAN_POINT('Ctrl Pts',(-1.43783746532133,-16.4279450992207,
7.));
#11912=CARTESIAN_POINT('Ctrl Pts',(-1.43783746532133,-16.4279450992207,
-1.39999999999999));
#11913=CARTESIAN_POINT('Ctrl Pts',(-1.3620126454106,-16.3372938385016,7.));
#11914=CARTESIAN_POINT('Ctrl Pts',(-1.3620126454106,-16.3372938385016,-1.39999999999999));
#11915=CARTESIAN_POINT('Ctrl Pts',(-1.23650382033378,-16.2452435266959,
7.));
#11916=CARTESIAN_POINT('Ctrl Pts',(-1.23650382033378,-16.2452435266959,
-1.39999999999999));
#11917=CARTESIAN_POINT('Ctrl Pts',(-1.1199417984865,-16.2167242606458,7.));
#11918=CARTESIAN_POINT('Ctrl Pts',(-1.1199417984865,-16.2167242606458,-1.39999999999999));
#11919=CARTESIAN_POINT('Ctrl Pts',(-1.04967429885986,-16.2160625265911,
7.));
#11920=CARTESIAN_POINT('Ctrl Pts',(-1.04967429885986,-16.2160625265911,
-1.39999999999999));
#11921=CARTESIAN_POINT('',(-1.04967429885986,-16.2160625265911,7.));
#11922=CARTESIAN_POINT('Origin',(0.,0.,7.));
#11923=CARTESIAN_POINT('',(1.04967429885974,-16.2160625265911,7.));
#11924=CARTESIAN_POINT('Ctrl Pts',(1.04967429885983,-16.2160625265911,7.));
#11925=CARTESIAN_POINT('Ctrl Pts',(1.04967429885983,-16.2160625265911,-1.4));
#11926=CARTESIAN_POINT('Ctrl Pts',(1.11994179848648,-16.2167242606459,7.));
#11927=CARTESIAN_POINT('Ctrl Pts',(1.11994179848648,-16.2167242606459,-1.4));
#11928=CARTESIAN_POINT('Ctrl Pts',(1.23650382033375,-16.2452435266959,7.));
#11929=CARTESIAN_POINT('Ctrl Pts',(1.23650382033375,-16.2452435266959,-1.4));
#11930=CARTESIAN_POINT('Ctrl Pts',(1.36201264541055,-16.3372938385016,7.));
#11931=CARTESIAN_POINT('Ctrl Pts',(1.36201264541055,-16.3372938385016,-1.4));
#11932=CARTESIAN_POINT('Ctrl Pts',(1.4378374653213,-16.4279450992208,7.));
#11933=CARTESIAN_POINT('Ctrl Pts',(1.4378374653213,-16.4279450992208,-1.4));
#11934=CARTESIAN_POINT('Ctrl Pts',(1.4905179616981,-16.5198135565978,7.));
#11935=CARTESIAN_POINT('Ctrl Pts',(1.4905179616981,-16.5198135565978,-1.4));
#11936=CARTESIAN_POINT('Ctrl Pts',(1.52918899676862,-16.6138949491149,7.));
#11937=CARTESIAN_POINT('Ctrl Pts',(1.52918899676862,-16.6138949491149,-1.4));
#11938=CARTESIAN_POINT('Ctrl Pts',(1.55162638755016,-16.6896454316359,7.));
#11939=CARTESIAN_POINT('Ctrl Pts',(1.55162638755016,-16.6896454316359,-1.4));
#11940=CARTESIAN_POINT('Ctrl Pts',(1.56489594057218,-16.7455711436431,7.));
#11941=CARTESIAN_POINT('Ctrl Pts',(1.56489594057218,-16.7455711436431,-1.4));
#11942=CARTESIAN_POINT('Ctrl Pts',(1.57225556404312,-16.7804505865492,7.));
#11943=CARTESIAN_POINT('Ctrl Pts',(1.57225556404312,-16.7804505865492,-1.4));
#11944=CARTESIAN_POINT('Ctrl Pts',(1.57930034717562,-16.8195656763126,7.));
#11945=CARTESIAN_POINT('Ctrl Pts',(1.57930034717562,-16.8195656763126,-1.4));
#11946=CARTESIAN_POINT('Ctrl Pts',(1.58971419725804,-16.8793055486399,7.));
#11947=CARTESIAN_POINT('Ctrl Pts',(1.58971419725804,-16.8793055486399,-1.4));
#11948=CARTESIAN_POINT('Ctrl Pts',(1.60803840593144,-16.9659973771906,7.));
#11949=CARTESIAN_POINT('Ctrl Pts',(1.60803840593144,-16.9659973771906,-1.4));
#11950=CARTESIAN_POINT('Ctrl Pts',(1.6370032466926,-17.0826338282622,7.));
#11951=CARTESIAN_POINT('Ctrl Pts',(1.6370032466926,-17.0826338282622,-1.4));
#11952=CARTESIAN_POINT('Ctrl Pts',(1.67639424155263,-17.2191007779953,7.));
#11953=CARTESIAN_POINT('Ctrl Pts',(1.67639424155263,-17.2191007779953,-1.4));
#11954=CARTESIAN_POINT('Ctrl Pts',(1.72763282051121,-17.3747717371572,7.));
#11955=CARTESIAN_POINT('Ctrl Pts',(1.72763282051121,-17.3747717371572,-1.4));
#11956=CARTESIAN_POINT('Ctrl Pts',(1.79222730418269,-17.548917731071,7.));
#11957=CARTESIAN_POINT('Ctrl Pts',(1.79222730418269,-17.548917731071,-1.4));
#11958=CARTESIAN_POINT('Ctrl Pts',(1.87160676754277,-17.7407325407201,7.));
#11959=CARTESIAN_POINT('Ctrl Pts',(1.87160676754277,-17.7407325407201,-1.4));
#11960=CARTESIAN_POINT('Ctrl Pts',(1.96717098182925,-17.949326772361,7.));
#11961=CARTESIAN_POINT('Ctrl Pts',(1.96717098182925,-17.949326772361,-1.4));
#11962=CARTESIAN_POINT('Ctrl Pts',(2.08026807216972,-18.1737325312257,7.));
#11963=CARTESIAN_POINT('Ctrl Pts',(2.08026807216972,-18.1737325312257,-1.4));
#11964=CARTESIAN_POINT('Ctrl Pts',(2.2465324944921,-18.4751451900744,7.));
#11965=CARTESIAN_POINT('Ctrl Pts',(2.2465324944921,-18.4751451900744,-1.4));
#11966=CARTESIAN_POINT('Ctrl Pts',(2.38389175781394,-18.6965496529788,7.));
#11967=CARTESIAN_POINT('Ctrl Pts',(2.38389175781394,-18.6965496529788,-1.4));
#11968=CARTESIAN_POINT('Ctrl Pts',(2.47738131311187,-18.8377966288376,7.));
#11969=CARTESIAN_POINT('Ctrl Pts',(2.47738131311187,-18.8377966288376,-1.4));
#11970=CARTESIAN_POINT('',(2.47738131311187,-18.8377966288376,7.));
#11971=CARTESIAN_POINT('Origin',(0.,0.,7.));
#11972=CARTESIAN_POINT('',(3.46506965370692,-18.6813621637974,7.));
#11973=CARTESIAN_POINT('Ctrl Pts',(3.46506965370701,-18.6813621637973,7.));
#11974=CARTESIAN_POINT('Ctrl Pts',(3.46506965370701,-18.6813621637973,-1.39999999999999));
#11975=CARTESIAN_POINT('Ctrl Pts',(3.51033578853419,-18.5181384456162,7.));
#11976=CARTESIAN_POINT('Ctrl Pts',(3.51033578853419,-18.5181384456162,-1.39999999999999));
#11977=CARTESIAN_POINT('Ctrl Pts',(3.57255446932203,-18.2651239417329,7.));
#11978=CARTESIAN_POINT('Ctrl Pts',(3.57255446932203,-18.2651239417329,-1.39999999999999));
#11979=CARTESIAN_POINT('Ctrl Pts',(3.63753969769579,-17.9270849363835,7.));
#11980=CARTESIAN_POINT('Ctrl Pts',(3.63753969769579,-17.9270849363835,-1.39999999999999));
#11981=CARTESIAN_POINT('Ctrl Pts',(3.67575622931334,-17.6787134541915,7.));
#11982=CARTESIAN_POINT('Ctrl Pts',(3.67575622931334,-17.6787134541915,-1.39999999999999));
#11983=CARTESIAN_POINT('Ctrl Pts',(3.7021840355295,-17.4507975846592,7.));
#11984=CARTESIAN_POINT('Ctrl Pts',(3.7021840355295,-17.4507975846592,-1.39999999999999));
#11985=CARTESIAN_POINT('Ctrl Pts',(3.71840435546372,-17.2438412568379,7.));
#11986=CARTESIAN_POINT('Ctrl Pts',(3.71840435546372,-17.2438412568379,-1.39999999999999));
#11987=CARTESIAN_POINT('Ctrl Pts',(3.72602328845457,-17.0582577813421,7.));
#11988=CARTESIAN_POINT('Ctrl Pts',(3.72602328845457,-17.0582577813421,-1.39999999999999));
#11989=CARTESIAN_POINT('Ctrl Pts',(3.72664910094712,-16.8943723095674,7.));
#11990=CARTESIAN_POINT('Ctrl Pts',(3.72664910094712,-16.8943723095674,-1.39999999999999));
#11991=CARTESIAN_POINT('Ctrl Pts',(3.72194155665404,-16.7524120409277,7.));
#11992=CARTESIAN_POINT('Ctrl Pts',(3.72194155665404,-16.7524120409277,-1.39999999999999));
#11993=CARTESIAN_POINT('Ctrl Pts',(3.71344611165872,-16.632533556064,7.));
#11994=CARTESIAN_POINT('Ctrl Pts',(3.71344611165872,-16.632533556064,-1.39999999999999));
#11995=CARTESIAN_POINT('Ctrl Pts',(3.70408422142791,-16.5444222357228,7.));
#11996=CARTESIAN_POINT('Ctrl Pts',(3.70408422142791,-16.5444222357228,-1.39999999999999));
#11997=CARTESIAN_POINT('Ctrl Pts',(3.69552774561757,-16.4843881842109,7.));
#11998=CARTESIAN_POINT('Ctrl Pts',(3.69552774561757,-16.4843881842109,-1.39999999999999));
#11999=CARTESIAN_POINT('Ctrl Pts',(3.69014050504827,-16.4450105654963,7.));
#12000=CARTESIAN_POINT('Ctrl Pts',(3.69014050504827,-16.4450105654963,-1.39999999999999));
#12001=CARTESIAN_POINT('Ctrl Pts',(3.68636158229547,-16.409563995311,7.));
#12002=CARTESIAN_POINT('Ctrl Pts',(3.68636158229547,-16.409563995311,-1.39999999999999));
#12003=CARTESIAN_POINT('Ctrl Pts',(3.68169968173261,-16.3522749650865,7.));
#12004=CARTESIAN_POINT('Ctrl Pts',(3.68169968173261,-16.3522749650865,-1.39999999999999));
#12005=CARTESIAN_POINT('Ctrl Pts',(3.67963072201297,-16.2732984400115,7.));
#12006=CARTESIAN_POINT('Ctrl Pts',(3.67963072201297,-16.2732984400115,-1.39999999999999));
#12007=CARTESIAN_POINT('Ctrl Pts',(3.68733631276642,-16.1718717115691,7.));
#12008=CARTESIAN_POINT('Ctrl Pts',(3.68733631276642,-16.1718717115691,-1.39999999999999));
#12009=CARTESIAN_POINT('Ctrl Pts',(3.70904952755071,-16.0682204478862,7.));
#12010=CARTESIAN_POINT('Ctrl Pts',(3.70904952755071,-16.0682204478862,-1.39999999999999));
#12011=CARTESIAN_POINT('Ctrl Pts',(3.75315043649999,-15.958574817721,7.));
#12012=CARTESIAN_POINT('Ctrl Pts',(3.75315043649999,-15.958574817721,-1.39999999999999));
#12013=CARTESIAN_POINT('Ctrl Pts',(3.84407131175639,-15.8322454089585,7.));
#12014=CARTESIAN_POINT('Ctrl Pts',(3.84407131175639,-15.8322454089585,-1.39999999999999));
#12015=CARTESIAN_POINT('Ctrl Pts',(3.94611544431021,-15.7691023294921,7.));
#12016=CARTESIAN_POINT('Ctrl Pts',(3.94611544431021,-15.7691023294921,-1.39999999999999));
#12017=CARTESIAN_POINT('Ctrl Pts',(4.01273932064523,-15.7467591314704,7.));
#12018=CARTESIAN_POINT('Ctrl Pts',(4.01273932064523,-15.7467591314704,-1.39999999999999));
#12019=CARTESIAN_POINT('',(4.01273932064523,-15.7467591314704,7.));
#12020=CARTESIAN_POINT('Origin',(0.,0.,7.));
#12021=CARTESIAN_POINT('',(6.00933848448151,-15.0980247376579,7.));
#12022=CARTESIAN_POINT('Ctrl Pts',(6.00933848448159,-15.0980247376579,7.));
#12023=CARTESIAN_POINT('Ctrl Pts',(6.00933848448159,-15.0980247376579,-1.4));
#12024=CARTESIAN_POINT('Ctrl Pts',(6.07637133495396,-15.0769402326058,7.));
#12025=CARTESIAN_POINT('Ctrl Pts',(6.07637133495396,-15.0769402326058,-1.4));
#12026=CARTESIAN_POINT('Ctrl Pts',(6.1960413432609,-15.0680440207731,7.));
#12027=CARTESIAN_POINT('Ctrl Pts',(6.1960413432609,-15.0680440207731,-1.4));
#12028=CARTESIAN_POINT('Ctrl Pts',(6.34385243988821,-15.1168047097502,7.));
#12029=CARTESIAN_POINT('Ctrl Pts',(6.34385243988821,-15.1168047097502,-1.4));
#12030=CARTESIAN_POINT('Ctrl Pts',(6.44397890908497,-15.1795880240196,7.));
#12031=CARTESIAN_POINT('Ctrl Pts',(6.44397890908497,-15.1795880240196,-1.4));
#12032=CARTESIAN_POINT('Ctrl Pts',(6.52246995302229,-15.2506809503975,7.));
#12033=CARTESIAN_POINT('Ctrl Pts',(6.52246995302229,-15.2506809503975,-1.4));
#12034=CARTESIAN_POINT('Ctrl Pts',(6.58832104206024,-15.3282076647862,7.));
#12035=CARTESIAN_POINT('Ctrl Pts',(6.58832104206024,-15.3282076647862,-1.4));
#12036=CARTESIAN_POINT('Ctrl Pts',(6.63306845520277,-15.3933171197393,7.));
#12037=CARTESIAN_POINT('Ctrl Pts',(6.63306845520277,-15.3933171197393,-1.4));
#12038=CARTESIAN_POINT('Ctrl Pts',(6.66297054550544,-15.4424051151807,7.));
#12039=CARTESIAN_POINT('Ctrl Pts',(6.66297054550544,-15.4424051151807,-1.4));
#12040=CARTESIAN_POINT('Ctrl Pts',(6.68074830397727,-15.4733031879166,7.));
#12041=CARTESIAN_POINT('Ctrl Pts',(6.68074830397727,-15.4733031879166,-1.4));
#12042=CARTESIAN_POINT('Ctrl Pts',(6.69953551835471,-15.5083268912119,7.));
#12043=CARTESIAN_POINT('Ctrl Pts',(6.69953551835471,-15.5083268912119,-1.4));
#12044=CARTESIAN_POINT('Ctrl Pts',(6.72790031412625,-15.5619248294191,7.));
#12045=CARTESIAN_POINT('Ctrl Pts',(6.72790031412625,-15.5619248294191,-1.4));
#12046=CARTESIAN_POINT('Ctrl Pts',(6.77211692048664,-15.6387111659832,7.));
#12047=CARTESIAN_POINT('Ctrl Pts',(6.77211692048664,-15.6387111659832,-1.4));
#12048=CARTESIAN_POINT('Ctrl Pts',(6.83570676658069,-15.7406883947778,7.));
#12049=CARTESIAN_POINT('Ctrl Pts',(6.83570676658069,-15.7406883947778,-1.4));
#12050=CARTESIAN_POINT('Ctrl Pts',(6.91534043556371,-15.8583036897433,7.));
#12051=CARTESIAN_POINT('Ctrl Pts',(6.91534043556371,-15.8583036897433,-1.4));
#12052=CARTESIAN_POINT('Ctrl Pts',(7.01217619187964,-15.9905219781863,7.));
#12053=CARTESIAN_POINT('Ctrl Pts',(7.01217619187964,-15.9905219781863,-1.4));
#12054=CARTESIAN_POINT('Ctrl Pts',(7.12742326811382,-16.1361838672874,7.));
#12055=CARTESIAN_POINT('Ctrl Pts',(7.12742326811382,-16.1361838672874,-1.4));
#12056=CARTESIAN_POINT('Ctrl Pts',(7.2621916599568,-16.2940809887434,7.));
#12057=CARTESIAN_POINT('Ctrl Pts',(7.2621916599568,-16.2940809887434,-1.4));
#12058=CARTESIAN_POINT('Ctrl Pts',(7.41753779118422,-16.4629349257385,7.));
#12059=CARTESIAN_POINT('Ctrl Pts',(7.41753779118422,-16.4629349257385,-1.4));
#12060=CARTESIAN_POINT('Ctrl Pts',(7.59444470905135,-16.6414085620714,7.));
#12061=CARTESIAN_POINT('Ctrl Pts',(7.59444470905135,-16.6414085620714,-1.4));
#12062=CARTESIAN_POINT('Ctrl Pts',(7.84571320523309,-16.8766905033058,7.));
#12063=CARTESIAN_POINT('Ctrl Pts',(7.84571320523309,-16.8766905033058,-1.4));
#12064=CARTESIAN_POINT('Ctrl Pts',(8.04476736935673,-17.0448123137865,7.));
#12065=CARTESIAN_POINT('Ctrl Pts',(8.04476736935673,-17.0448123137865,-1.4));
#12066=CARTESIAN_POINT('Ctrl Pts',(8.17732893607279,-17.1502563092004,7.));
#12067=CARTESIAN_POINT('Ctrl Pts',(8.17732893607279,-17.1502563092004,-1.4));
#12068=CARTESIAN_POINT('',(8.17732893607279,-17.1502563092004,7.));
#12069=CARTESIAN_POINT('Origin',(0.,0.,7.));
#12070=CARTESIAN_POINT('',(9.06833546026109,-16.6962658094609,7.));
#12071=CARTESIAN_POINT('Ctrl Pts',(9.06833546026116,-16.6962658094608,7.));
#12072=CARTESIAN_POINT('Ctrl Pts',(9.06833546026116,-16.6962658094608,-1.39999999999999));
#12073=CARTESIAN_POINT('Ctrl Pts',(9.06094720995301,-16.5270428237395,7.));
#12074=CARTESIAN_POINT('Ctrl Pts',(9.06094720995301,-16.5270428237395,-1.39999999999999));
#12075=CARTESIAN_POINT('Ctrl Pts',(9.0419349102283,-16.267185101373,7.));
#12076=CARTESIAN_POINT('Ctrl Pts',(9.0419349102283,-16.267185101373,-1.39999999999999));
#12077=CARTESIAN_POINT('Ctrl Pts',(8.99927973772149,-15.9256093626227,7.));
#12078=CARTESIAN_POINT('Ctrl Pts',(8.99927973772149,-15.9256093626227,-1.39999999999999));
#12079=CARTESIAN_POINT('Ctrl Pts',(8.95887481023114,-15.6775844882862,7.));
#12080=CARTESIAN_POINT('Ctrl Pts',(8.95887481023114,-15.6775844882862,-1.39999999999999));
#12081=CARTESIAN_POINT('Ctrl Pts',(8.91357927057119,-15.4526569741556,7.));
#12082=CARTESIAN_POINT('Ctrl Pts',(8.91357927057119,-15.4526569741556,-1.39999999999999));
#12083=CARTESIAN_POINT('Ctrl Pts',(8.8650526891508,-15.2508174554787,7.));
#12084=CARTESIAN_POINT('Ctrl Pts',(8.8650526891508,-15.2508174554787,-1.39999999999999));
#12085=CARTESIAN_POINT('Ctrl Pts',(8.81495027721559,-15.0719627020186,7.));
#12086=CARTESIAN_POINT('Ctrl Pts',(8.81495027721559,-15.0719627020186,-1.39999999999999));
#12087=CARTESIAN_POINT('Ctrl Pts',(8.76490206435508,-14.9159049694657,7.));
#12088=CARTESIAN_POINT('Ctrl Pts',(8.76490206435508,-14.9159049694657,-1.39999999999999));
#12089=CARTESIAN_POINT('Ctrl Pts',(8.7165567881437,-14.7823474421092,7.));
#12090=CARTESIAN_POINT('Ctrl Pts',(8.7165567881437,-14.7823474421092,-1.39999999999999));
#12091=CARTESIAN_POINT('Ctrl Pts',(8.67143265073927,-14.6709614647944,7.));
#12092=CARTESIAN_POINT('Ctrl Pts',(8.67143265073927,-14.6709614647944,-1.39999999999999));
#12093=CARTESIAN_POINT('Ctrl Pts',(8.63530106864817,-14.5900556026053,7.));
#12094=CARTESIAN_POINT('Ctrl Pts',(8.63530106864817,-14.5900556026053,-1.39999999999999));
#12095=CARTESIAN_POINT('Ctrl Pts',(8.60861183441386,-14.5356039231526,7.));
#12096=CARTESIAN_POINT('Ctrl Pts',(8.60861183441386,-14.5356039231526,-1.39999999999999));
#12097=CARTESIAN_POINT('Ctrl Pts',(8.59131991078477,-14.4998183311667,7.));
#12098=CARTESIAN_POINT('Ctrl Pts',(8.59131991078477,-14.4998183311667,-1.39999999999999));
#12099=CARTESIAN_POINT('Ctrl Pts',(8.57677234909656,-14.4672743909626,7.));
#12100=CARTESIAN_POINT('Ctrl Pts',(8.57677234909656,-14.4672743909626,-1.39999999999999));
#12101=CARTESIAN_POINT('Ctrl Pts',(8.55463533425731,-14.4142298919554,7.));
#12102=CARTESIAN_POINT('Ctrl Pts',(8.55463533425731,-14.4142298919554,-1.39999999999999));
#12103=CARTESIAN_POINT('Ctrl Pts',(8.52826254822914,-14.3397580968625,7.));
#12104=CARTESIAN_POINT('Ctrl Pts',(8.52826254822914,-14.3397580968625,-1.39999999999999));
#12105=CARTESIAN_POINT('Ctrl Pts',(8.50424841775455,-14.2409143873564,7.));
#12106=CARTESIAN_POINT('Ctrl Pts',(8.50424841775455,-14.2409143873564,-1.39999999999999));
#12107=CARTESIAN_POINT('Ctrl Pts',(8.49286891019841,-14.1356264252376,7.));
#12108=CARTESIAN_POINT('Ctrl Pts',(8.49286891019841,-14.1356264252376,-1.39999999999999));
#12109=CARTESIAN_POINT('Ctrl Pts',(8.50092900394917,-14.0177193038531,7.));
#12110=CARTESIAN_POINT('Ctrl Pts',(8.50092900394917,-14.0177193038531,-1.39999999999999));
#12111=CARTESIAN_POINT('Ctrl Pts',(8.54836196063206,-13.8694768008521,7.));
#12112=CARTESIAN_POINT('Ctrl Pts',(8.54836196063206,-13.8694768008521,-1.39999999999999));
#12113=CARTESIAN_POINT('Ctrl Pts',(8.62589941321478,-13.7778907925312,7.));
#12114=CARTESIAN_POINT('Ctrl Pts',(8.62589941321478,-13.7778907925312,-1.39999999999999));
#12115=CARTESIAN_POINT('Ctrl Pts',(8.68235805704667,-13.7360532384392,7.));
#12116=CARTESIAN_POINT('Ctrl Pts',(8.68235805704667,-13.7360532384392,-1.39999999999999));
#12117=CARTESIAN_POINT('',(8.68235805704667,-13.7360532384392,7.));
#12118=CARTESIAN_POINT('Origin',(0.,0.,7.));
#12119=CARTESIAN_POINT('',(10.3807667497191,-12.5020870932787,7.));
#12120=CARTESIAN_POINT('Ctrl Pts',(10.3807667497191,-12.5020870932787,7.));
#12121=CARTESIAN_POINT('Ctrl Pts',(10.3807667497191,-12.5020870932787,-1.4));
#12122=CARTESIAN_POINT('Ctrl Pts',(10.4380033085876,-12.4613202473788,7.));
#12123=CARTESIAN_POINT('Ctrl Pts',(10.4380033085876,-12.4613202473788,-1.4));
#12124=CARTESIAN_POINT('Ctrl Pts',(10.5490671691512,-12.4158793808611,7.));
#12125=CARTESIAN_POINT('Ctrl Pts',(10.5490671691512,-12.4158793808611,-1.4));
#12126=CARTESIAN_POINT('Ctrl Pts',(10.7047117573306,-12.4165774110367,7.));
#12127=CARTESIAN_POINT('Ctrl Pts',(10.7047117573306,-12.4165774110367,-1.4));
#12128=CARTESIAN_POINT('Ctrl Pts',(10.8193387993863,-12.4453471106188,7.));
#12129=CARTESIAN_POINT('Ctrl Pts',(10.8193387993863,-12.4453471106188,-1.4));
#12130=CARTESIAN_POINT('Ctrl Pts',(10.9159571406243,-12.48870543503,7.));
#12131=CARTESIAN_POINT('Ctrl Pts',(10.9159571406243,-12.48870543503,-1.4));
#12132=CARTESIAN_POINT('Ctrl Pts',(11.0025423202231,-12.5420886163255,7.));
#12133=CARTESIAN_POINT('Ctrl Pts',(11.0025423202231,-12.5420886163255,-1.4));
#12134=CARTESIAN_POINT('Ctrl Pts',(11.0652195671547,-12.5901836766158,7.));
#12135=CARTESIAN_POINT('Ctrl Pts',(11.0652195671547,-12.5901836766158,-1.4));
#12136=CARTESIAN_POINT('Ctrl Pts',(11.1088271697991,-12.6276288804813,7.));
#12137=CARTESIAN_POINT('Ctrl Pts',(11.1088271697991,-12.6276288804813,-1.4));
#12138=CARTESIAN_POINT('Ctrl Pts',(11.1352828524077,-12.651521064408,7.));
#12139=CARTESIAN_POINT('Ctrl Pts',(11.1352828524077,-12.651521064408,-1.4));
#12140=CARTESIAN_POINT('Ctrl Pts',(11.1639734745885,-12.6790250171322,7.));
#12141=CARTESIAN_POINT('Ctrl Pts',(11.1639734745885,-12.6790250171322,-1.4));
#12142=CARTESIAN_POINT('Ctrl Pts',(11.2075126722099,-12.7212344815888,7.));
#12143=CARTESIAN_POINT('Ctrl Pts',(11.2075126722099,-12.7212344815888,-1.4));
#12144=CARTESIAN_POINT('Ctrl Pts',(11.2732934467515,-12.7805989445416,7.));
#12145=CARTESIAN_POINT('Ctrl Pts',(11.2732934467515,-12.7805989445416,-1.4));
#12146=CARTESIAN_POINT('Ctrl Pts',(11.3652836809863,-12.8579347093876,7.));
#12147=CARTESIAN_POINT('Ctrl Pts',(11.3652836809863,-12.8579347093876,-1.4));
#12148=CARTESIAN_POINT('Ctrl Pts',(11.4773649257318,-12.9451853450404,7.));
#12149=CARTESIAN_POINT('Ctrl Pts',(11.4773649257318,-12.9451853450404,-1.4));
#12150=CARTESIAN_POINT('Ctrl Pts',(11.6103189008825,-13.0410085154727,7.));
#12151=CARTESIAN_POINT('Ctrl Pts',(11.6103189008825,-13.0410085154727,-1.4));
#12152=CARTESIAN_POINT('Ctrl Pts',(11.764937382884,-13.1439278991698,7.));
#12153=CARTESIAN_POINT('Ctrl Pts',(11.764937382884,-13.1439278991698,-1.4));
#12154=CARTESIAN_POINT('Ctrl Pts',(11.9419026340297,-13.2524512620507,7.));
#12155=CARTESIAN_POINT('Ctrl Pts',(11.9419026340297,-13.2524512620507,-1.4));
#12156=CARTESIAN_POINT('Ctrl Pts',(12.1418243205134,-13.3650363045724,7.));
#12157=CARTESIAN_POINT('Ctrl Pts',(12.1418243205134,-13.3650363045724,-1.4));
#12158=CARTESIAN_POINT('Ctrl Pts',(12.3652241842034,-13.4801075753502,7.));
#12159=CARTESIAN_POINT('Ctrl Pts',(12.3652241842034,-13.4801075753502,-1.4));
#12160=CARTESIAN_POINT('Ctrl Pts',(12.6769008431476,-13.6262277632565,7.));
#12161=CARTESIAN_POINT('Ctrl Pts',(12.6769008431476,-13.6262277632565,-1.4));
#12162=CARTESIAN_POINT('Ctrl Pts',(12.9181650995967,-13.7246099871303,7.));
#12163=CARTESIAN_POINT('Ctrl Pts',(12.9181650995967,-13.7246099871303,-1.4));
#12164=CARTESIAN_POINT('Ctrl Pts',(13.07682262797,-13.7839294091566,7.));
#12165=CARTESIAN_POINT('Ctrl Pts',(13.07682262797,-13.7839294091566,-1.4));
#12166=CARTESIAN_POINT('',(13.07682262797,-13.7839294091566,7.));
#12167=CARTESIAN_POINT('Origin',(0.,1.10390771809154E-15,7.));
#12168=CARTESIAN_POINT('',(13.7839294091565,-13.0768226279701,7.));
#12169=CARTESIAN_POINT('Ctrl Pts',(13.7839294091566,-13.07682262797,7.));
#12170=CARTESIAN_POINT('Ctrl Pts',(13.7839294091566,-13.07682262797,-1.39999999999999));
#12171=CARTESIAN_POINT('Ctrl Pts',(13.7246099871302,-12.9181650995967,7.));
#12172=CARTESIAN_POINT('Ctrl Pts',(13.7246099871302,-12.9181650995967,-1.39999999999999));
#12173=CARTESIAN_POINT('Ctrl Pts',(13.6262277632565,-12.6769008431476,7.));
#12174=CARTESIAN_POINT('Ctrl Pts',(13.6262277632565,-12.6769008431476,-1.39999999999999));
#12175=CARTESIAN_POINT('Ctrl Pts',(13.4801075753502,-12.3652241842034,7.));
#12176=CARTESIAN_POINT('Ctrl Pts',(13.4801075753502,-12.3652241842034,-1.39999999999999));
#12177=CARTESIAN_POINT('Ctrl Pts',(13.3650363045723,-12.1418243205134,7.));
#12178=CARTESIAN_POINT('Ctrl Pts',(13.3650363045723,-12.1418243205134,-1.39999999999999));
#12179=CARTESIAN_POINT('Ctrl Pts',(13.2524512620508,-11.9419026340297,7.));
#12180=CARTESIAN_POINT('Ctrl Pts',(13.2524512620508,-11.9419026340297,-1.39999999999999));
#12181=CARTESIAN_POINT('Ctrl Pts',(13.1439278991698,-11.764937382884,7.));
#12182=CARTESIAN_POINT('Ctrl Pts',(13.1439278991698,-11.764937382884,-1.39999999999999));
#12183=CARTESIAN_POINT('Ctrl Pts',(13.0410085154728,-11.6103189008825,7.));
#12184=CARTESIAN_POINT('Ctrl Pts',(13.0410085154728,-11.6103189008825,-1.39999999999999));
#12185=CARTESIAN_POINT('Ctrl Pts',(12.9451853450404,-11.4773649257318,7.));
#12186=CARTESIAN_POINT('Ctrl Pts',(12.9451853450404,-11.4773649257318,-1.39999999999999));
#12187=CARTESIAN_POINT('Ctrl Pts',(12.8579347093876,-11.3652836809863,7.));
#12188=CARTESIAN_POINT('Ctrl Pts',(12.8579347093876,-11.3652836809863,-1.39999999999999));
#12189=CARTESIAN_POINT('Ctrl Pts',(12.7805989445416,-11.2732934467515,7.));
#12190=CARTESIAN_POINT('Ctrl Pts',(12.7805989445416,-11.2732934467515,-1.39999999999999));
#12191=CARTESIAN_POINT('Ctrl Pts',(12.7212344815888,-11.2075126722099,7.));
#12192=CARTESIAN_POINT('Ctrl Pts',(12.7212344815888,-11.2075126722099,-1.39999999999999));
#12193=CARTESIAN_POINT('Ctrl Pts',(12.6790250171322,-11.1639734745885,7.));
#12194=CARTESIAN_POINT('Ctrl Pts',(12.6790250171322,-11.1639734745885,-1.39999999999999));
#12195=CARTESIAN_POINT('Ctrl Pts',(12.6515210644081,-11.1352828524076,7.));
#12196=CARTESIAN_POINT('Ctrl Pts',(12.6515210644081,-11.1352828524076,-1.39999999999999));
#12197=CARTESIAN_POINT('Ctrl Pts',(12.6276288804813,-11.108827169799,7.));
#12198=CARTESIAN_POINT('Ctrl Pts',(12.6276288804813,-11.108827169799,-1.39999999999999));
#12199=CARTESIAN_POINT('Ctrl Pts',(12.5901836766158,-11.0652195671547,7.));
#12200=CARTESIAN_POINT('Ctrl Pts',(12.5901836766158,-11.0652195671547,-1.39999999999999));
#12201=CARTESIAN_POINT('Ctrl Pts',(12.5420886163255,-11.0025423202231,7.));
#12202=CARTESIAN_POINT('Ctrl Pts',(12.5420886163255,-11.0025423202231,-1.39999999999999));
#12203=CARTESIAN_POINT('Ctrl Pts',(12.48870543503,-10.9159571406243,7.));
#12204=CARTESIAN_POINT('Ctrl Pts',(12.48870543503,-10.9159571406243,-1.39999999999999));
#12205=CARTESIAN_POINT('Ctrl Pts',(12.4453471106188,-10.8193387993863,7.));
#12206=CARTESIAN_POINT('Ctrl Pts',(12.4453471106188,-10.8193387993863,-1.39999999999999));
#12207=CARTESIAN_POINT('Ctrl Pts',(12.4165774110367,-10.7047117573306,7.));
#12208=CARTESIAN_POINT('Ctrl Pts',(12.4165774110367,-10.7047117573306,-1.39999999999999));
#12209=CARTESIAN_POINT('Ctrl Pts',(12.4158793808611,-10.5490671691512,7.));
#12210=CARTESIAN_POINT('Ctrl Pts',(12.4158793808611,-10.5490671691512,-1.39999999999999));
#12211=CARTESIAN_POINT('Ctrl Pts',(12.4613202473788,-10.4380033085876,7.));
#12212=CARTESIAN_POINT('Ctrl Pts',(12.4613202473788,-10.4380033085876,-1.39999999999999));
#12213=CARTESIAN_POINT('Ctrl Pts',(12.5020870932787,-10.3807667497191,7.));
#12214=CARTESIAN_POINT('Ctrl Pts',(12.5020870932787,-10.3807667497191,-1.39999999999999));
#12215=CARTESIAN_POINT('',(12.5020870932787,-10.3807667497191,7.));
#12216=CARTESIAN_POINT('Origin',(0.,0.,7.));
#12217=CARTESIAN_POINT('',(13.7360532384392,-8.68235805704669,7.));
#12218=CARTESIAN_POINT('Ctrl Pts',(13.7360532384392,-8.68235805704669,7.));
#12219=CARTESIAN_POINT('Ctrl Pts',(13.7360532384392,-8.68235805704669,-1.39999999999998));
#12220=CARTESIAN_POINT('Ctrl Pts',(13.7778907925313,-8.62589941321482,7.));
#12221=CARTESIAN_POINT('Ctrl Pts',(13.7778907925313,-8.62589941321482,-1.39999999999998));
#12222=CARTESIAN_POINT('Ctrl Pts',(13.8694768008521,-8.54836196063209,7.));
#12223=CARTESIAN_POINT('Ctrl Pts',(13.8694768008521,-8.54836196063209,-1.39999999999998));
#12224=CARTESIAN_POINT('Ctrl Pts',(14.0177193038531,-8.50092900394922,7.));
#12225=CARTESIAN_POINT('Ctrl Pts',(14.0177193038531,-8.50092900394922,-1.39999999999998));
#12226=CARTESIAN_POINT('Ctrl Pts',(14.1356264252377,-8.49286891019844,7.));
#12227=CARTESIAN_POINT('Ctrl Pts',(14.1356264252377,-8.49286891019844,-1.39999999999998));
#12228=CARTESIAN_POINT('Ctrl Pts',(14.2409143873564,-8.50424841775457,7.));
#12229=CARTESIAN_POINT('Ctrl Pts',(14.2409143873564,-8.50424841775457,-1.39999999999998));
#12230=CARTESIAN_POINT('Ctrl Pts',(14.3397580968626,-8.52826254822916,7.));
#12231=CARTESIAN_POINT('Ctrl Pts',(14.3397580968626,-8.52826254822916,-1.39999999999998));
#12232=CARTESIAN_POINT('Ctrl Pts',(14.4142298919554,-8.55463533425733,7.));
#12233=CARTESIAN_POINT('Ctrl Pts',(14.4142298919554,-8.55463533425733,-1.39999999999998));
#12234=CARTESIAN_POINT('Ctrl Pts',(14.4672743909627,-8.57677234909657,7.));
#12235=CARTESIAN_POINT('Ctrl Pts',(14.4672743909627,-8.57677234909657,-1.39999999999998));
#12236=CARTESIAN_POINT('Ctrl Pts',(14.4998183311667,-8.59131991078477,7.));
#12237=CARTESIAN_POINT('Ctrl Pts',(14.4998183311667,-8.59131991078477,-1.39999999999998));
#12238=CARTESIAN_POINT('Ctrl Pts',(14.5356039231527,-8.6086118344139,7.));
#12239=CARTESIAN_POINT('Ctrl Pts',(14.5356039231527,-8.6086118344139,-1.39999999999998));
#12240=CARTESIAN_POINT('Ctrl Pts',(14.5900556026053,-8.63530106864818,7.));
#12241=CARTESIAN_POINT('Ctrl Pts',(14.5900556026053,-8.63530106864818,-1.39999999999998));
#12242=CARTESIAN_POINT('Ctrl Pts',(14.6709614647944,-8.67143265073928,7.));
#12243=CARTESIAN_POINT('Ctrl Pts',(14.6709614647944,-8.67143265073928,-1.39999999999998));
#12244=CARTESIAN_POINT('Ctrl Pts',(14.7823474421092,-8.71655678814373,7.));
#12245=CARTESIAN_POINT('Ctrl Pts',(14.7823474421092,-8.71655678814373,-1.39999999999998));
#12246=CARTESIAN_POINT('Ctrl Pts',(14.9159049694657,-8.7649020643551,7.));
#12247=CARTESIAN_POINT('Ctrl Pts',(14.9159049694657,-8.7649020643551,-1.39999999999998));
#12248=CARTESIAN_POINT('Ctrl Pts',(15.0719627020186,-8.81495027721557,7.));
#12249=CARTESIAN_POINT('Ctrl Pts',(15.0719627020186,-8.81495027721557,-1.39999999999998));
#12250=CARTESIAN_POINT('Ctrl Pts',(15.2508174554788,-8.86505268915084,7.));
#12251=CARTESIAN_POINT('Ctrl Pts',(15.2508174554788,-8.86505268915084,-1.39999999999998));
#12252=CARTESIAN_POINT('Ctrl Pts',(15.4526569741556,-8.91357927057117,7.));
#12253=CARTESIAN_POINT('Ctrl Pts',(15.4526569741556,-8.91357927057117,-1.39999999999998));
#12254=CARTESIAN_POINT('Ctrl Pts',(15.6775844882862,-8.95887481023116,7.));
#12255=CARTESIAN_POINT('Ctrl Pts',(15.6775844882862,-8.95887481023116,-1.39999999999998));
#12256=CARTESIAN_POINT('Ctrl Pts',(15.9256093626227,-8.99927973772153,7.));
#12257=CARTESIAN_POINT('Ctrl Pts',(15.9256093626227,-8.99927973772153,-1.39999999999998));
#12258=CARTESIAN_POINT('Ctrl Pts',(16.2671851013731,-9.04193491022831,7.));
#12259=CARTESIAN_POINT('Ctrl Pts',(16.2671851013731,-9.04193491022831,-1.39999999999998));
#12260=CARTESIAN_POINT('Ctrl Pts',(16.5270428237395,-9.06094720995305,7.));
#12261=CARTESIAN_POINT('Ctrl Pts',(16.5270428237395,-9.06094720995305,-1.39999999999998));
#12262=CARTESIAN_POINT('Ctrl Pts',(16.6962658094608,-9.06833546026116,7.));
#12263=CARTESIAN_POINT('Ctrl Pts',(16.6962658094608,-9.06833546026116,-1.39999999999998));
#12264=CARTESIAN_POINT('',(16.6962658094608,-9.06833546026116,7.));
#12265=CARTESIAN_POINT('Origin',(0.,0.,7.));
#12266=CARTESIAN_POINT('',(17.1502563092003,-8.17732893607285,7.));
#12267=CARTESIAN_POINT('Ctrl Pts',(17.1502563092004,-8.17732893607279,7.));
#12268=CARTESIAN_POINT('Ctrl Pts',(17.1502563092004,-8.17732893607279,-1.39999999999999));
#12269=CARTESIAN_POINT('Ctrl Pts',(17.0448123137865,-8.04476736935674,7.));
#12270=CARTESIAN_POINT('Ctrl Pts',(17.0448123137865,-8.04476736935674,-1.39999999999999));
#12271=CARTESIAN_POINT('Ctrl Pts',(16.8766905033057,-7.84571320523309,7.));
#12272=CARTESIAN_POINT('Ctrl Pts',(16.8766905033057,-7.84571320523309,-1.39999999999999));
#12273=CARTESIAN_POINT('Ctrl Pts',(16.6414085620714,-7.59444470905136,7.));
#12274=CARTESIAN_POINT('Ctrl Pts',(16.6414085620714,-7.59444470905136,-1.39999999999999));
#12275=CARTESIAN_POINT('Ctrl Pts',(16.4629349257385,-7.41753779118421,7.));
#12276=CARTESIAN_POINT('Ctrl Pts',(16.4629349257385,-7.41753779118421,-1.39999999999999));
#12277=CARTESIAN_POINT('Ctrl Pts',(16.2940809887434,-7.26219165995679,7.));
#12278=CARTESIAN_POINT('Ctrl Pts',(16.2940809887434,-7.26219165995679,-1.39999999999999));
#12279=CARTESIAN_POINT('Ctrl Pts',(16.1361838672874,-7.12742326811383,7.));
#12280=CARTESIAN_POINT('Ctrl Pts',(16.1361838672874,-7.12742326811383,-1.39999999999999));
#12281=CARTESIAN_POINT('Ctrl Pts',(15.9905219781863,-7.01217619187962,7.));
#12282=CARTESIAN_POINT('Ctrl Pts',(15.9905219781863,-7.01217619187962,-1.39999999999999));
#12283=CARTESIAN_POINT('Ctrl Pts',(15.8583036897433,-6.91534043556369,7.));
#12284=CARTESIAN_POINT('Ctrl Pts',(15.8583036897433,-6.91534043556369,-1.39999999999999));
#12285=CARTESIAN_POINT('Ctrl Pts',(15.7406883947777,-6.83570676658069,7.));
#12286=CARTESIAN_POINT('Ctrl Pts',(15.7406883947777,-6.83570676658069,-1.39999999999999));
#12287=CARTESIAN_POINT('Ctrl Pts',(15.6387111659832,-6.77211692048663,7.));
#12288=CARTESIAN_POINT('Ctrl Pts',(15.6387111659832,-6.77211692048663,-1.39999999999999));
#12289=CARTESIAN_POINT('Ctrl Pts',(15.5619248294191,-6.72790031412624,7.));
#12290=CARTESIAN_POINT('Ctrl Pts',(15.5619248294191,-6.72790031412624,-1.39999999999999));
#12291=CARTESIAN_POINT('Ctrl Pts',(15.5083268912119,-6.69953551835472,7.));
#12292=CARTESIAN_POINT('Ctrl Pts',(15.5083268912119,-6.69953551835472,-1.39999999999999));
#12293=CARTESIAN_POINT('Ctrl Pts',(15.4733031879166,-6.68074830397725,7.));
#12294=CARTESIAN_POINT('Ctrl Pts',(15.4733031879166,-6.68074830397725,-1.39999999999999));
#12295=CARTESIAN_POINT('Ctrl Pts',(15.4424051151807,-6.66297054550541,7.));
#12296=CARTESIAN_POINT('Ctrl Pts',(15.4424051151807,-6.66297054550541,-1.39999999999999));
#12297=CARTESIAN_POINT('Ctrl Pts',(15.3933171197393,-6.63306845520276,7.));
#12298=CARTESIAN_POINT('Ctrl Pts',(15.3933171197393,-6.63306845520276,-1.39999999999999));
#12299=CARTESIAN_POINT('Ctrl Pts',(15.3282076647862,-6.58832104206022,7.));
#12300=CARTESIAN_POINT('Ctrl Pts',(15.3282076647862,-6.58832104206022,-1.39999999999999));
#12301=CARTESIAN_POINT('Ctrl Pts',(15.2506809503975,-6.52246995302226,7.));
#12302=CARTESIAN_POINT('Ctrl Pts',(15.2506809503975,-6.52246995302226,-1.39999999999999));
#12303=CARTESIAN_POINT('Ctrl Pts',(15.1795880240196,-6.44397890908496,7.));
#12304=CARTESIAN_POINT('Ctrl Pts',(15.1795880240196,-6.44397890908496,-1.39999999999999));
#12305=CARTESIAN_POINT('Ctrl Pts',(15.1168047097501,-6.34385243988822,7.));
#12306=CARTESIAN_POINT('Ctrl Pts',(15.1168047097501,-6.34385243988822,-1.39999999999999));
#12307=CARTESIAN_POINT('Ctrl Pts',(15.0680440207731,-6.1960413432609,7.));
#12308=CARTESIAN_POINT('Ctrl Pts',(15.0680440207731,-6.1960413432609,-1.39999999999999));
#12309=CARTESIAN_POINT('Ctrl Pts',(15.0769402326058,-6.07637133495394,7.));
#12310=CARTESIAN_POINT('Ctrl Pts',(15.0769402326058,-6.07637133495394,-1.39999999999999));
#12311=CARTESIAN_POINT('Ctrl Pts',(15.0980247376579,-6.00933848448159,7.));
#12312=CARTESIAN_POINT('Ctrl Pts',(15.0980247376579,-6.00933848448159,-1.39999999999999));
#12313=CARTESIAN_POINT('',(15.0980247376579,-6.00933848448159,7.));
#12314=CARTESIAN_POINT('Origin',(0.,0.,7.));
#12315=CARTESIAN_POINT('',(15.7467591314704,-4.01273932064523,7.));
#12316=CARTESIAN_POINT('Ctrl Pts',(15.7467591314704,-4.01273932064524,7.));
#12317=CARTESIAN_POINT('Ctrl Pts',(15.7467591314704,-4.01273932064524,-1.4));
#12318=CARTESIAN_POINT('Ctrl Pts',(15.7691023294921,-3.94611544431022,7.));
#12319=CARTESIAN_POINT('Ctrl Pts',(15.7691023294921,-3.94611544431022,-1.4));
#12320=CARTESIAN_POINT('Ctrl Pts',(15.8322454089585,-3.8440713117564,7.));
#12321=CARTESIAN_POINT('Ctrl Pts',(15.8322454089585,-3.8440713117564,-1.4));
#12322=CARTESIAN_POINT('Ctrl Pts',(15.958574817721,-3.75315043650002,7.));
#12323=CARTESIAN_POINT('Ctrl Pts',(15.958574817721,-3.75315043650002,-1.4));
#12324=CARTESIAN_POINT('Ctrl Pts',(16.0682204478862,-3.70904952755073,7.));
#12325=CARTESIAN_POINT('Ctrl Pts',(16.0682204478862,-3.70904952755073,-1.4));
#12326=CARTESIAN_POINT('Ctrl Pts',(16.1718717115691,-3.68733631276642,7.));
#12327=CARTESIAN_POINT('Ctrl Pts',(16.1718717115691,-3.68733631276642,-1.4));
#12328=CARTESIAN_POINT('Ctrl Pts',(16.2732984400115,-3.67963072201298,7.));
#12329=CARTESIAN_POINT('Ctrl Pts',(16.2732984400115,-3.67963072201298,-1.4));
#12330=CARTESIAN_POINT('Ctrl Pts',(16.3522749650865,-3.68169968173262,7.));
#12331=CARTESIAN_POINT('Ctrl Pts',(16.3522749650865,-3.68169968173262,-1.4));
#12332=CARTESIAN_POINT('Ctrl Pts',(16.409563995311,-3.68636158229546,7.));
#12333=CARTESIAN_POINT('Ctrl Pts',(16.409563995311,-3.68636158229546,-1.4));
#12334=CARTESIAN_POINT('Ctrl Pts',(16.4450105654963,-3.69014050504826,7.));
#12335=CARTESIAN_POINT('Ctrl Pts',(16.4450105654963,-3.69014050504826,-1.4));
#12336=CARTESIAN_POINT('Ctrl Pts',(16.4843881842109,-3.6955277456176,7.));
#12337=CARTESIAN_POINT('Ctrl Pts',(16.4843881842109,-3.6955277456176,-1.4));
#12338=CARTESIAN_POINT('Ctrl Pts',(16.5444222357228,-3.70408422142792,7.));
#12339=CARTESIAN_POINT('Ctrl Pts',(16.5444222357228,-3.70408422142792,-1.4));
#12340=CARTESIAN_POINT('Ctrl Pts',(16.632533556064,-3.71344611165872,7.));
#12341=CARTESIAN_POINT('Ctrl Pts',(16.632533556064,-3.71344611165872,-1.4));
#12342=CARTESIAN_POINT('Ctrl Pts',(16.7524120409277,-3.72194155665406,7.));
#12343=CARTESIAN_POINT('Ctrl Pts',(16.7524120409277,-3.72194155665406,-1.4));
#12344=CARTESIAN_POINT('Ctrl Pts',(16.8943723095674,-3.72664910094713,7.));
#12345=CARTESIAN_POINT('Ctrl Pts',(16.8943723095674,-3.72664910094713,-1.4));
#12346=CARTESIAN_POINT('Ctrl Pts',(17.0582577813421,-3.72602328845455,7.));
#12347=CARTESIAN_POINT('Ctrl Pts',(17.0582577813421,-3.72602328845455,-1.4));
#12348=CARTESIAN_POINT('Ctrl Pts',(17.2438412568379,-3.71840435546376,7.));
#12349=CARTESIAN_POINT('Ctrl Pts',(17.2438412568379,-3.71840435546376,-1.4));
#12350=CARTESIAN_POINT('Ctrl Pts',(17.4507975846592,-3.70218403552949,7.));
#12351=CARTESIAN_POINT('Ctrl Pts',(17.4507975846592,-3.70218403552949,-1.4));
#12352=CARTESIAN_POINT('Ctrl Pts',(17.6787134541915,-3.67575622931335,7.));
#12353=CARTESIAN_POINT('Ctrl Pts',(17.6787134541915,-3.67575622931335,-1.4));
#12354=CARTESIAN_POINT('Ctrl Pts',(17.9270849363835,-3.63753969769582,7.));
#12355=CARTESIAN_POINT('Ctrl Pts',(17.9270849363835,-3.63753969769582,-1.4));
#12356=CARTESIAN_POINT('Ctrl Pts',(18.265123941733,-3.57255446932205,7.));
#12357=CARTESIAN_POINT('Ctrl Pts',(18.265123941733,-3.57255446932205,-1.4));
#12358=CARTESIAN_POINT('Ctrl Pts',(18.5181384456163,-3.51033578853422,7.));
#12359=CARTESIAN_POINT('Ctrl Pts',(18.5181384456163,-3.51033578853422,-1.4));
#12360=CARTESIAN_POINT('Ctrl Pts',(18.6813621637973,-3.46506965370701,7.));
#12361=CARTESIAN_POINT('Ctrl Pts',(18.6813621637973,-3.46506965370701,-1.4));
#12362=CARTESIAN_POINT('',(18.6813621637973,-3.46506965370701,7.));
#12363=CARTESIAN_POINT('Origin',(0.,0.,7.));
#12364=CARTESIAN_POINT('',(18.8377966288376,-2.47738131311191,7.));
#12365=CARTESIAN_POINT('Ctrl Pts',(18.8377966288376,-2.47738131311187,7.));
#12366=CARTESIAN_POINT('Ctrl Pts',(18.8377966288376,-2.47738131311187,-1.39999999999999));
#12367=CARTESIAN_POINT('Ctrl Pts',(18.6965496529788,-2.38389175781396,7.));
#12368=CARTESIAN_POINT('Ctrl Pts',(18.6965496529788,-2.38389175781396,-1.39999999999999));
#12369=CARTESIAN_POINT('Ctrl Pts',(18.4751451900744,-2.24653249449211,7.));
#12370=CARTESIAN_POINT('Ctrl Pts',(18.4751451900744,-2.24653249449211,-1.39999999999999));
#12371=CARTESIAN_POINT('Ctrl Pts',(18.1737325312257,-2.08026807216974,7.));
#12372=CARTESIAN_POINT('Ctrl Pts',(18.1737325312257,-2.08026807216974,-1.39999999999999));
#12373=CARTESIAN_POINT('Ctrl Pts',(17.949326772361,-1.96717098182924,7.));
#12374=CARTESIAN_POINT('Ctrl Pts',(17.949326772361,-1.96717098182924,-1.39999999999999));
#12375=CARTESIAN_POINT('Ctrl Pts',(17.7407325407201,-1.87160676754275,7.));
#12376=CARTESIAN_POINT('Ctrl Pts',(17.7407325407201,-1.87160676754275,-1.39999999999999));
#12377=CARTESIAN_POINT('Ctrl Pts',(17.548917731071,-1.7922273041827,7.));
#12378=CARTESIAN_POINT('Ctrl Pts',(17.548917731071,-1.7922273041827,-1.39999999999999));
#12379=CARTESIAN_POINT('Ctrl Pts',(17.3747717371572,-1.72763282051117,7.));
#12380=CARTESIAN_POINT('Ctrl Pts',(17.3747717371572,-1.72763282051117,-1.39999999999999));
#12381=CARTESIAN_POINT('Ctrl Pts',(17.2191007779952,-1.67639424155261,7.));
#12382=CARTESIAN_POINT('Ctrl Pts',(17.2191007779952,-1.67639424155261,-1.39999999999999));
#12383=CARTESIAN_POINT('Ctrl Pts',(17.0826338282621,-1.6370032466926,7.));
#12384=CARTESIAN_POINT('Ctrl Pts',(17.0826338282621,-1.6370032466926,-1.39999999999999));
#12385=CARTESIAN_POINT('Ctrl Pts',(16.9659973771906,-1.60803840593143,7.));
#12386=CARTESIAN_POINT('Ctrl Pts',(16.9659973771906,-1.60803840593143,-1.39999999999999));
#12387=CARTESIAN_POINT('Ctrl Pts',(16.8793055486399,-1.58971419725802,7.));
#12388=CARTESIAN_POINT('Ctrl Pts',(16.8793055486399,-1.58971419725802,-1.39999999999999));
#12389=CARTESIAN_POINT('Ctrl Pts',(16.8195656763126,-1.57930034717563,7.));
#12390=CARTESIAN_POINT('Ctrl Pts',(16.8195656763126,-1.57930034717563,-1.39999999999999));
#12391=CARTESIAN_POINT('Ctrl Pts',(16.7804505865492,-1.57225556404309,7.));
#12392=CARTESIAN_POINT('Ctrl Pts',(16.7804505865492,-1.57225556404309,-1.39999999999999));
#12393=CARTESIAN_POINT('Ctrl Pts',(16.7455711436431,-1.56489594057215,7.));
#12394=CARTESIAN_POINT('Ctrl Pts',(16.7455711436431,-1.56489594057215,-1.39999999999999));
#12395=CARTESIAN_POINT('Ctrl Pts',(16.6896454316358,-1.55162638755015,7.));
#12396=CARTESIAN_POINT('Ctrl Pts',(16.6896454316358,-1.55162638755015,-1.39999999999999));
#12397=CARTESIAN_POINT('Ctrl Pts',(16.6138949491149,-1.5291889967686,7.));
#12398=CARTESIAN_POINT('Ctrl Pts',(16.6138949491149,-1.5291889967686,-1.39999999999999));
#12399=CARTESIAN_POINT('Ctrl Pts',(16.5198135565977,-1.49051796169807,7.));
#12400=CARTESIAN_POINT('Ctrl Pts',(16.5198135565977,-1.49051796169807,-1.39999999999999));
#12401=CARTESIAN_POINT('Ctrl Pts',(16.4279450992207,-1.43783746532129,7.));
#12402=CARTESIAN_POINT('Ctrl Pts',(16.4279450992207,-1.43783746532129,-1.39999999999999));
#12403=CARTESIAN_POINT('Ctrl Pts',(16.3372938385016,-1.36201264541057,7.));
#12404=CARTESIAN_POINT('Ctrl Pts',(16.3372938385016,-1.36201264541057,-1.39999999999999));
#12405=CARTESIAN_POINT('Ctrl Pts',(16.2452435266959,-1.23650382033374,7.));
#12406=CARTESIAN_POINT('Ctrl Pts',(16.2452435266959,-1.23650382033374,-1.39999999999999));
#12407=CARTESIAN_POINT('Ctrl Pts',(16.2167242606458,-1.11994179848647,7.));
#12408=CARTESIAN_POINT('Ctrl Pts',(16.2167242606458,-1.11994179848647,-1.39999999999999));
#12409=CARTESIAN_POINT('Ctrl Pts',(16.2160625265911,-1.04967429885982,7.));
#12410=CARTESIAN_POINT('Ctrl Pts',(16.2160625265911,-1.04967429885982,-1.39999999999999));
#12411=CARTESIAN_POINT('',(16.2160625265911,-1.04967429885982,7.));
#12412=CARTESIAN_POINT('Origin',(0.,0.,7.));
#12413=CARTESIAN_POINT('',(16.2160625265911,1.0496742988598,7.));
#12414=CARTESIAN_POINT('Ctrl Pts',(16.2160625265911,1.04967429885982,7.));
#12415=CARTESIAN_POINT('Ctrl Pts',(16.2160625265911,1.04967429885982,-1.4));
#12416=CARTESIAN_POINT('Ctrl Pts',(16.2167242606459,1.11994179848647,7.));
#12417=CARTESIAN_POINT('Ctrl Pts',(16.2167242606459,1.11994179848647,-1.4));
#12418=CARTESIAN_POINT('Ctrl Pts',(16.2452435266959,1.23650382033374,7.));
#12419=CARTESIAN_POINT('Ctrl Pts',(16.2452435266959,1.23650382033374,-1.4));
#12420=CARTESIAN_POINT('Ctrl Pts',(16.3372938385016,1.36201264541054,7.));
#12421=CARTESIAN_POINT('Ctrl Pts',(16.3372938385016,1.36201264541054,-1.4));
#12422=CARTESIAN_POINT('Ctrl Pts',(16.4279450992208,1.43783746532129,7.));
#12423=CARTESIAN_POINT('Ctrl Pts',(16.4279450992208,1.43783746532129,-1.4));
#12424=CARTESIAN_POINT('Ctrl Pts',(16.5198135565978,1.49051796169809,7.));
#12425=CARTESIAN_POINT('Ctrl Pts',(16.5198135565978,1.49051796169809,-1.4));
#12426=CARTESIAN_POINT('Ctrl Pts',(16.6138949491149,1.52918899676861,7.));
#12427=CARTESIAN_POINT('Ctrl Pts',(16.6138949491149,1.52918899676861,-1.4));
#12428=CARTESIAN_POINT('Ctrl Pts',(16.6896454316359,1.55162638755015,7.));
#12429=CARTESIAN_POINT('Ctrl Pts',(16.6896454316359,1.55162638755015,-1.4));
#12430=CARTESIAN_POINT('Ctrl Pts',(16.7455711436431,1.56489594057217,7.));
#12431=CARTESIAN_POINT('Ctrl Pts',(16.7455711436431,1.56489594057217,-1.4));
#12432=CARTESIAN_POINT('Ctrl Pts',(16.7804505865492,1.57225556404311,7.));
#12433=CARTESIAN_POINT('Ctrl Pts',(16.7804505865492,1.57225556404311,-1.4));
#12434=CARTESIAN_POINT('Ctrl Pts',(16.8195656763126,1.57930034717561,7.));
#12435=CARTESIAN_POINT('Ctrl Pts',(16.8195656763126,1.57930034717561,-1.4));
#12436=CARTESIAN_POINT('Ctrl Pts',(16.8793055486399,1.58971419725803,7.));
#12437=CARTESIAN_POINT('Ctrl Pts',(16.8793055486399,1.58971419725803,-1.4));
#12438=CARTESIAN_POINT('Ctrl Pts',(16.9659973771906,1.60803840593143,7.));
#12439=CARTESIAN_POINT('Ctrl Pts',(16.9659973771906,1.60803840593143,-1.4));
#12440=CARTESIAN_POINT('Ctrl Pts',(17.0826338282621,1.63700324669259,7.));
#12441=CARTESIAN_POINT('Ctrl Pts',(17.0826338282621,1.63700324669259,-1.4));
#12442=CARTESIAN_POINT('Ctrl Pts',(17.2191007779953,1.67639424155262,7.));
#12443=CARTESIAN_POINT('Ctrl Pts',(17.2191007779953,1.67639424155262,-1.4));
#12444=CARTESIAN_POINT('Ctrl Pts',(17.3747717371572,1.7276328205112,7.));
#12445=CARTESIAN_POINT('Ctrl Pts',(17.3747717371572,1.7276328205112,-1.4));
#12446=CARTESIAN_POINT('Ctrl Pts',(17.548917731071,1.79222730418268,7.));
#12447=CARTESIAN_POINT('Ctrl Pts',(17.548917731071,1.79222730418268,-1.4));
#12448=CARTESIAN_POINT('Ctrl Pts',(17.7407325407201,1.87160676754277,7.));
#12449=CARTESIAN_POINT('Ctrl Pts',(17.7407325407201,1.87160676754277,-1.4));
#12450=CARTESIAN_POINT('Ctrl Pts',(17.949326772361,1.96717098182924,7.));
#12451=CARTESIAN_POINT('Ctrl Pts',(17.949326772361,1.96717098182924,-1.4));
#12452=CARTESIAN_POINT('Ctrl Pts',(18.1737325312257,2.08026807216972,7.));
#12453=CARTESIAN_POINT('Ctrl Pts',(18.1737325312257,2.08026807216972,-1.4));
#12454=CARTESIAN_POINT('Ctrl Pts',(18.4751451900744,2.2465324944921,7.));
#12455=CARTESIAN_POINT('Ctrl Pts',(18.4751451900744,2.2465324944921,-1.4));
#12456=CARTESIAN_POINT('Ctrl Pts',(18.6965496529788,2.38389175781394,7.));
#12457=CARTESIAN_POINT('Ctrl Pts',(18.6965496529788,2.38389175781394,-1.4));
#12458=CARTESIAN_POINT('Ctrl Pts',(18.8377966288376,2.47738131311188,7.));
#12459=CARTESIAN_POINT('Ctrl Pts',(18.8377966288376,2.47738131311188,-1.4));
#12460=CARTESIAN_POINT('',(18.8377966288376,2.47738131311188,7.));
#12461=CARTESIAN_POINT('Origin',(1.73472347597681E-15,0.,7.));
#12462=CARTESIAN_POINT('',(18.6813621637973,3.46506965370699,7.));
#12463=CARTESIAN_POINT('Ctrl Pts',(18.6813621637973,3.46506965370701,7.));
#12464=CARTESIAN_POINT('Ctrl Pts',(18.6813621637973,3.46506965370701,-1.39999999999999));
#12465=CARTESIAN_POINT('Ctrl Pts',(18.5181384456162,3.51033578853419,7.));
#12466=CARTESIAN_POINT('Ctrl Pts',(18.5181384456162,3.51033578853419,-1.39999999999999));
#12467=CARTESIAN_POINT('Ctrl Pts',(18.2651239417329,3.57255446932204,7.));
#12468=CARTESIAN_POINT('Ctrl Pts',(18.2651239417329,3.57255446932204,-1.39999999999999));
#12469=CARTESIAN_POINT('Ctrl Pts',(17.9270849363835,3.63753969769579,7.));
#12470=CARTESIAN_POINT('Ctrl Pts',(17.9270849363835,3.63753969769579,-1.39999999999999));
#12471=CARTESIAN_POINT('Ctrl Pts',(17.6787134541915,3.67575622931334,7.));
#12472=CARTESIAN_POINT('Ctrl Pts',(17.6787134541915,3.67575622931334,-1.39999999999999));
#12473=CARTESIAN_POINT('Ctrl Pts',(17.4507975846592,3.70218403552951,7.));
#12474=CARTESIAN_POINT('Ctrl Pts',(17.4507975846592,3.70218403552951,-1.39999999999999));
#12475=CARTESIAN_POINT('Ctrl Pts',(17.2438412568379,3.71840435546372,7.));
#12476=CARTESIAN_POINT('Ctrl Pts',(17.2438412568379,3.71840435546372,-1.39999999999999));
#12477=CARTESIAN_POINT('Ctrl Pts',(17.0582577813421,3.72602328845457,7.));
#12478=CARTESIAN_POINT('Ctrl Pts',(17.0582577813421,3.72602328845457,-1.39999999999999));
#12479=CARTESIAN_POINT('Ctrl Pts',(16.8943723095674,3.72664910094712,7.));
#12480=CARTESIAN_POINT('Ctrl Pts',(16.8943723095674,3.72664910094712,-1.39999999999999));
#12481=CARTESIAN_POINT('Ctrl Pts',(16.7524120409277,3.72194155665404,7.));
#12482=CARTESIAN_POINT('Ctrl Pts',(16.7524120409277,3.72194155665404,-1.39999999999999));
#12483=CARTESIAN_POINT('Ctrl Pts',(16.632533556064,3.71344611165872,7.));
#12484=CARTESIAN_POINT('Ctrl Pts',(16.632533556064,3.71344611165872,-1.39999999999999));
#12485=CARTESIAN_POINT('Ctrl Pts',(16.5444222357228,3.70408422142792,7.));
#12486=CARTESIAN_POINT('Ctrl Pts',(16.5444222357228,3.70408422142792,-1.39999999999999));
#12487=CARTESIAN_POINT('Ctrl Pts',(16.4843881842109,3.69552774561757,7.));
#12488=CARTESIAN_POINT('Ctrl Pts',(16.4843881842109,3.69552774561757,-1.39999999999999));
#12489=CARTESIAN_POINT('Ctrl Pts',(16.4450105654963,3.69014050504827,7.));
#12490=CARTESIAN_POINT('Ctrl Pts',(16.4450105654963,3.69014050504827,-1.39999999999999));
#12491=CARTESIAN_POINT('Ctrl Pts',(16.409563995311,3.68636158229547,7.));
#12492=CARTESIAN_POINT('Ctrl Pts',(16.409563995311,3.68636158229547,-1.39999999999999));
#12493=CARTESIAN_POINT('Ctrl Pts',(16.3522749650865,3.68169968173261,7.));
#12494=CARTESIAN_POINT('Ctrl Pts',(16.3522749650865,3.68169968173261,-1.39999999999999));
#12495=CARTESIAN_POINT('Ctrl Pts',(16.2732984400115,3.67963072201297,7.));
#12496=CARTESIAN_POINT('Ctrl Pts',(16.2732984400115,3.67963072201297,-1.39999999999999));
#12497=CARTESIAN_POINT('Ctrl Pts',(16.1718717115691,3.68733631276642,7.));
#12498=CARTESIAN_POINT('Ctrl Pts',(16.1718717115691,3.68733631276642,-1.39999999999999));
#12499=CARTESIAN_POINT('Ctrl Pts',(16.0682204478862,3.70904952755071,7.));
#12500=CARTESIAN_POINT('Ctrl Pts',(16.0682204478862,3.70904952755071,-1.39999999999999));
#12501=CARTESIAN_POINT('Ctrl Pts',(15.958574817721,3.75315043649999,7.));
#12502=CARTESIAN_POINT('Ctrl Pts',(15.958574817721,3.75315043649999,-1.39999999999999));
#12503=CARTESIAN_POINT('Ctrl Pts',(15.8322454089585,3.84407131175639,7.));
#12504=CARTESIAN_POINT('Ctrl Pts',(15.8322454089585,3.84407131175639,-1.39999999999999));
#12505=CARTESIAN_POINT('Ctrl Pts',(15.7691023294921,3.94611544431022,7.));
#12506=CARTESIAN_POINT('Ctrl Pts',(15.7691023294921,3.94611544431022,-1.39999999999999));
#12507=CARTESIAN_POINT('Ctrl Pts',(15.7467591314704,4.01273932064524,7.));
#12508=CARTESIAN_POINT('Ctrl Pts',(15.7467591314704,4.01273932064524,-1.39999999999999));
#12509=CARTESIAN_POINT('',(15.7467591314704,4.01273932064524,7.));
#12510=CARTESIAN_POINT('Origin',(0.,0.,7.));
#12511=CARTESIAN_POINT('Origin',(0.,0.,6.));
#12512=CARTESIAN_POINT('Origin',(0.,0.,1.));
#12513=CARTESIAN_POINT('',(0.,0.,0.));
#12514=CARTESIAN_POINT('Origin',(25.,3.,-9.18485099360515E-15));
#12515=CARTESIAN_POINT('',(25.,3.,2.49999999999999));
#12516=CARTESIAN_POINT('Origin',(25.,3.,-9.18485099360515E-15));
#12517=CARTESIAN_POINT('',(25.,0.,2.49999999999999));
#12518=CARTESIAN_POINT('',(25.,3.,2.49999999999999));
#12519=CARTESIAN_POINT('Origin',(25.,0.,-9.18485099360515E-15));
#12520=CARTESIAN_POINT('Origin',(-25.,3.,0.));
#12521=CARTESIAN_POINT('',(-25.,3.,2.5));
#12522=CARTESIAN_POINT('Origin',(-25.,3.,0.));
#12523=CARTESIAN_POINT('',(-25.,0.,2.5));
#12524=CARTESIAN_POINT('',(-25.,3.,2.5));
#12525=CARTESIAN_POINT('Origin',(-25.,0.,0.));
#12526=CARTESIAN_POINT('Origin',(-25.,3.,0.));
#12527=CARTESIAN_POINT('',(-25.,3.,-5.));
#12528=CARTESIAN_POINT('',(-25.,3.,5.));
#12529=CARTESIAN_POINT('Origin',(-25.,3.,0.));
#12530=CARTESIAN_POINT('',(25.,3.,4.99999999999999));
#12531=CARTESIAN_POINT('',(-25.,3.,5.));
#12532=CARTESIAN_POINT('',(25.,3.,-5.00000000000001));
#12533=CARTESIAN_POINT('Origin',(25.,3.,-9.18485099360515E-15));
#12534=CARTESIAN_POINT('',(-25.,3.,-5.));
#12535=CARTESIAN_POINT('Origin',(-25.,0.,0.));
#12536=CARTESIAN_POINT('',(-25.,0.,-5.));
#12537=CARTESIAN_POINT('',(-25.,0.,5.));
#12538=CARTESIAN_POINT('Origin',(-25.,0.,0.));
#12539=CARTESIAN_POINT('',(25.,0.,-5.00000000000001));
#12540=CARTESIAN_POINT('',(-25.,0.,-5.));
#12541=CARTESIAN_POINT('',(25.,0.,4.99999999999999));
#12542=CARTESIAN_POINT('Origin',(25.,0.,-9.18485099360515E-15));
#12543=CARTESIAN_POINT('',(-25.,0.,5.));
#12544=CARTESIAN_POINT('Origin',(-25.,3.,0.));
#12545=CARTESIAN_POINT('',(-25.,3.,5.));
#12546=CARTESIAN_POINT('',(-25.,3.,-5.));
#12547=CARTESIAN_POINT('Origin',(-25.,3.,5.));
#12548=CARTESIAN_POINT('',(25.,3.,4.99999999999999));
#12549=CARTESIAN_POINT('Origin',(25.,3.,-9.18485099360515E-15));
#12550=CARTESIAN_POINT('',(25.,3.,-5.00000000000001));
#12551=CARTESIAN_POINT('Origin',(-25.,3.,-5.));
#12552=CARTESIAN_POINT('',(0.,0.,0.));
#12553=CARTESIAN_POINT('Origin',(-997.978312163513,0.,0.));
#12554=CARTESIAN_POINT('',(2.02168783648704,0.,0.));
#12555=CARTESIAN_POINT('',(1.30000000000002,0.,-1.25));
#12556=CARTESIAN_POINT('',(-997.978312163513,-2.12115047744979E-13,-1732.05080756886));
#12557=CARTESIAN_POINT('',(1.30000000000002,-1.08253175473055,-0.625000000000001));
#12558=CARTESIAN_POINT('Origin',(1.30000000000002,0.,0.));
#12559=CARTESIAN_POINT('',(1.30000000000002,-1.08253175473055,0.625000000000001));
#12560=CARTESIAN_POINT('Origin',(1.30000000000002,0.,0.));
#12561=CARTESIAN_POINT('',(1.30000000000002,0.,1.25));
#12562=CARTESIAN_POINT('Origin',(1.30000000000002,0.,0.));
#12563=CARTESIAN_POINT('',(1.30000000000002,1.08253175473055,0.625000000000001));
#12564=CARTESIAN_POINT('Origin',(1.30000000000002,0.,0.));
#12565=CARTESIAN_POINT('',(1.30000000000002,1.08253175473055,-0.625000000000001));
#12566=CARTESIAN_POINT('Origin',(1.30000000000002,0.,0.));
#12567=CARTESIAN_POINT('Origin',(1.30000000000002,0.,0.));
#12568=CARTESIAN_POINT('Origin',(2.40000000000001,0.,0.));
#12569=CARTESIAN_POINT('',(2.19999999999998,-2.69422295812418E-16,-2.2));
#12570=CARTESIAN_POINT('Origin',(2.19999999999998,0.,0.));
#12571=CARTESIAN_POINT('',(2.40000000000001,-2.44929359829471E-16,-2.));
#12572=CARTESIAN_POINT('Origin',(2.40000000000001,-2.69422295812418E-16,
-2.2));
#12573=CARTESIAN_POINT('Origin',(2.40000000000001,0.,0.));
#12574=CARTESIAN_POINT('Origin',(22.2,0.,0.));
#12575=CARTESIAN_POINT('',(21.81,-2.44929359829471E-16,-2.));
#12576=CARTESIAN_POINT('Origin',(21.81,0.,0.));
#12577=CARTESIAN_POINT('',(22.2,-1.97168134662724E-16,-1.61));
#12578=CARTESIAN_POINT('',(22.2,-1.97168134662724E-16,-1.61));
#12579=CARTESIAN_POINT('Origin',(22.2,0.,0.));
#12580=CARTESIAN_POINT('Origin',(0.,0.,0.));
#12581=CARTESIAN_POINT('',(0.,-2.44929359829471E-16,-2.));
#12582=CARTESIAN_POINT('Origin',(0.,0.,0.));
#12583=CARTESIAN_POINT('',(1.81999999999999,-4.65365783675994E-16,-3.8));
#12584=CARTESIAN_POINT('Origin',(1.81999999999999,0.,0.));
#12585=CARTESIAN_POINT('',(2.19999999999998,-4.65365783675994E-16,-3.8));
#12586=CARTESIAN_POINT('',(0.,-4.65365783675994E-16,-3.8));
#12587=CARTESIAN_POINT('Origin',(2.19999999999998,0.,0.));
#12588=CARTESIAN_POINT('Origin',(3.88527472527472,0.,0.));
#12589=CARTESIAN_POINT('',(0.,1.9,0.));
#12590=CARTESIAN_POINT('Origin',(0.,0.,0.));
#12591=CARTESIAN_POINT('Origin',(0.,0.,0.));
#12592=CARTESIAN_POINT('',(0.,0.721687836487033,1.25));
#12593=CARTESIAN_POINT('',(0.,-0.721687836487031,1.25));
#12594=CARTESIAN_POINT('',(0.,-0.721687836487031,1.25));
#12595=CARTESIAN_POINT('',(0.,-1.44337567297407,0.));
#12596=CARTESIAN_POINT('',(0.,-1.44337567297407,0.));
#12597=CARTESIAN_POINT('',(0.,-0.721687836487031,-1.25));
#12598=CARTESIAN_POINT('',(0.,-0.721687836487031,-1.25));
#12599=CARTESIAN_POINT('',(0.,0.721687836487033,-1.25));
#12600=CARTESIAN_POINT('',(0.,0.721687836487033,-1.25));
#12601=CARTESIAN_POINT('',(0.,1.44337567297407,0.));
#12602=CARTESIAN_POINT('',(0.,1.44337567297407,0.));
#12603=CARTESIAN_POINT('',(0.,0.721687836487033,1.25));
#12604=CARTESIAN_POINT('Origin',(2.19999999999998,2.,0.));
#12605=CARTESIAN_POINT('Origin',(22.2,0.,0.));
#12606=CARTESIAN_POINT('Origin',(1.30000000000002,-1.44337567297407,0.));
#12607=CARTESIAN_POINT('',(1.30000000000002,-0.721687836487031,1.25));
#12608=CARTESIAN_POINT('',(1.30000000000002,-1.44337567297407,0.));
#12609=CARTESIAN_POINT('',(1.30000000000002,-1.44337567297407,0.));
#12610=CARTESIAN_POINT('',(1.30000000000002,-1.44337567297407,0.));
#12611=CARTESIAN_POINT('',(1.30000000000002,-1.44337567297407,0.));
#12612=CARTESIAN_POINT('',(1.30000000000002,-0.721687836487031,1.25));
#12613=CARTESIAN_POINT('Origin',(1.30000000000002,-0.721687836487031,-1.25));
#12614=CARTESIAN_POINT('',(1.30000000000002,-0.721687836487031,-1.25));
#12615=CARTESIAN_POINT('',(1.30000000000002,-0.721687836487031,-1.25));
#12616=CARTESIAN_POINT('',(1.30000000000002,-0.721687836487031,-1.25));
#12617=CARTESIAN_POINT('',(1.30000000000002,-0.721687836487031,-1.25));
#12618=CARTESIAN_POINT('Origin',(1.30000000000002,0.721687836487033,-1.25));
#12619=CARTESIAN_POINT('',(1.30000000000002,0.721687836487033,-1.25));
#12620=CARTESIAN_POINT('',(1.30000000000002,0.721687836487033,-1.25));
#12621=CARTESIAN_POINT('',(1.30000000000002,0.721687836487033,-1.25));
#12622=CARTESIAN_POINT('',(1.30000000000002,0.721687836487033,-1.25));
#12623=CARTESIAN_POINT('Origin',(1.30000000000002,1.44337567297407,0.));
#12624=CARTESIAN_POINT('',(1.30000000000002,1.44337567297407,0.));
#12625=CARTESIAN_POINT('',(1.30000000000002,1.44337567297407,0.));
#12626=CARTESIAN_POINT('',(1.30000000000002,1.44337567297407,0.));
#12627=CARTESIAN_POINT('',(1.30000000000002,1.44337567297407,0.));
#12628=CARTESIAN_POINT('Origin',(1.30000000000002,0.721687836487033,1.25));
#12629=CARTESIAN_POINT('',(1.30000000000002,0.721687836487033,1.25));
#12630=CARTESIAN_POINT('',(1.30000000000002,0.721687836487033,1.25));
#12631=CARTESIAN_POINT('',(1.30000000000002,0.721687836487033,1.25));
#12632=CARTESIAN_POINT('',(1.30000000000002,0.721687836487033,1.25));
#12633=CARTESIAN_POINT('Origin',(1.30000000000002,-0.721687836487031,1.25));
#12634=CARTESIAN_POINT('',(1.30000000000002,-0.721687836487031,1.25));
#12635=CARTESIAN_POINT('',(1.30000000000002,-0.721687836487031,1.25));
#12636=CARTESIAN_POINT('Origin',(1.30000000000002,-1.44337567297406,0.));
#12637=CARTESIAN_POINT('Origin',(1.30000000000002,-1.44337567297406,0.));
#12638=CARTESIAN_POINT('Origin',(1.30000000000002,-1.44337567297406,0.));
#12639=CARTESIAN_POINT('Origin',(1.30000000000002,-1.44337567297406,0.));
#12640=CARTESIAN_POINT('Origin',(1.30000000000002,-1.44337567297406,0.));
#12641=CARTESIAN_POINT('Origin',(1.30000000000002,-1.44337567297406,0.));
#12642=CARTESIAN_POINT('',(0.,0.,0.));
#12643=CARTESIAN_POINT('Origin',(-997.978312163513,-2.97906491917051E-40,
0.));
#12644=CARTESIAN_POINT('',(2.02168783648704,0.,0.));
#12645=CARTESIAN_POINT('',(1.30000000000002,0.,-1.25));
#12646=CARTESIAN_POINT('',(-997.978312163513,-2.12115047744979E-13,-1732.05080756886));
#12647=CARTESIAN_POINT('',(1.30000000000002,-1.08253175473055,-0.624999999999987));
#12648=CARTESIAN_POINT('Origin',(1.30000000000002,0.,0.));
#12649=CARTESIAN_POINT('',(1.30000000000002,-1.08253175473055,0.624999999999987));
#12650=CARTESIAN_POINT('Origin',(1.30000000000002,0.,0.));
#12651=CARTESIAN_POINT('',(1.30000000000002,0.,1.25));
#12652=CARTESIAN_POINT('Origin',(1.30000000000002,0.,0.));
#12653=CARTESIAN_POINT('',(1.30000000000002,1.08253175473055,0.625000000000014));
#12654=CARTESIAN_POINT('Origin',(1.30000000000002,0.,0.));
#12655=CARTESIAN_POINT('',(1.30000000000002,1.08253175473055,-0.624999999999987));
#12656=CARTESIAN_POINT('Origin',(1.30000000000002,0.,0.));
#12657=CARTESIAN_POINT('Origin',(1.30000000000002,0.,0.));
#12658=CARTESIAN_POINT('Origin',(2.40000000000001,0.,0.));
#12659=CARTESIAN_POINT('',(2.19999999999998,-2.69422295812418E-16,-2.2));
#12660=CARTESIAN_POINT('Origin',(2.19999999999998,0.,0.));
#12661=CARTESIAN_POINT('',(2.40000000000001,-2.44929359829471E-16,-2.));
#12662=CARTESIAN_POINT('Origin',(2.40000000000001,-2.69422295812418E-16,
-2.2));
#12663=CARTESIAN_POINT('Origin',(2.40000000000001,0.,0.));
#12664=CARTESIAN_POINT('Origin',(10.2,0.,0.));
#12665=CARTESIAN_POINT('',(9.80999999999999,-2.44929359829471E-16,-2.));
#12666=CARTESIAN_POINT('Origin',(9.80999999999998,0.,0.));
#12667=CARTESIAN_POINT('',(10.2,-1.97168134662724E-16,-1.61));
#12668=CARTESIAN_POINT('',(10.2,-1.97168134662724E-16,-1.61));
#12669=CARTESIAN_POINT('Origin',(10.2,0.,0.));
#12670=CARTESIAN_POINT('Origin',(0.,0.,0.));
#12671=CARTESIAN_POINT('',(7.29660463542866E-59,-2.44929359829471E-16,-2.));
#12672=CARTESIAN_POINT('Origin',(0.,0.,0.));
#12673=CARTESIAN_POINT('',(1.81999999999999,-4.65365783675994E-16,-3.8));
#12674=CARTESIAN_POINT('Origin',(1.81999999999999,0.,0.));
#12675=CARTESIAN_POINT('',(2.19999999999998,-4.65365783675994E-16,-3.8));
#12676=CARTESIAN_POINT('',(1.38635488073145E-58,-4.65365783675994E-16,-3.8));
#12677=CARTESIAN_POINT('Origin',(2.19999999999998,0.,0.));
#12678=CARTESIAN_POINT('Origin',(3.88527472527472,0.,0.));
#12679=CARTESIAN_POINT('',(-5.66022334642396E-43,1.9,0.));
#12680=CARTESIAN_POINT('Origin',(0.,0.,0.));
#12681=CARTESIAN_POINT('Origin',(0.,0.,0.));
#12682=CARTESIAN_POINT('',(0.,0.721687836487031,1.25));
#12683=CARTESIAN_POINT('',(0.,-0.721687836487031,1.25));
#12684=CARTESIAN_POINT('',(0.,-0.721687836487031,1.25));
#12685=CARTESIAN_POINT('',(0.,-1.44337567297407,0.));
#12686=CARTESIAN_POINT('',(0.,-1.44337567297407,0.));
#12687=CARTESIAN_POINT('',(0.,-0.721687836487031,-1.25));
#12688=CARTESIAN_POINT('',(0.,-0.721687836487031,-1.25));
#12689=CARTESIAN_POINT('',(0.,0.721687836487031,-1.25));
#12690=CARTESIAN_POINT('',(0.,0.721687836487031,-1.25));
#12691=CARTESIAN_POINT('',(0.,1.44337567297407,0.));
#12692=CARTESIAN_POINT('',(0.,1.44337567297407,0.));
#12693=CARTESIAN_POINT('',(0.,0.721687836487031,1.25));
#12694=CARTESIAN_POINT('Origin',(2.19999999999998,2.,0.));
#12695=CARTESIAN_POINT('Origin',(10.2,0.,0.));
#12696=CARTESIAN_POINT('Origin',(1.30000000000002,-1.44337567297407,0.));
#12697=CARTESIAN_POINT('',(1.30000000000002,-0.721687836487031,1.25));
#12698=CARTESIAN_POINT('',(1.30000000000002,-1.44337567297407,0.));
#12699=CARTESIAN_POINT('',(1.30000000000002,-1.44337567297407,0.));
#12700=CARTESIAN_POINT('',(1.30000000000002,-1.44337567297407,0.));
#12701=CARTESIAN_POINT('',(1.30000000000002,-1.44337567297407,0.));
#12702=CARTESIAN_POINT('',(1.30000000000002,-0.721687836487031,1.25));
#12703=CARTESIAN_POINT('Origin',(1.30000000000002,-0.721687836487031,-1.25));
#12704=CARTESIAN_POINT('',(1.30000000000002,-0.721687836487031,-1.25));
#12705=CARTESIAN_POINT('',(1.30000000000002,-0.721687836487031,-1.25));
#12706=CARTESIAN_POINT('',(1.30000000000002,-0.721687836487031,-1.25));
#12707=CARTESIAN_POINT('',(1.30000000000002,-0.721687836487031,-1.25));
#12708=CARTESIAN_POINT('Origin',(1.30000000000002,0.721687836487031,-1.25));
#12709=CARTESIAN_POINT('',(1.30000000000002,0.721687836487031,-1.25));
#12710=CARTESIAN_POINT('',(1.30000000000002,0.721687836487031,-1.25));
#12711=CARTESIAN_POINT('',(1.30000000000002,0.721687836487031,-1.25));
#12712=CARTESIAN_POINT('',(1.30000000000002,0.721687836487031,-1.25));
#12713=CARTESIAN_POINT('Origin',(1.30000000000002,1.44337567297407,0.));
#12714=CARTESIAN_POINT('',(1.30000000000002,1.44337567297407,0.));
#12715=CARTESIAN_POINT('',(1.30000000000002,1.44337567297407,0.));
#12716=CARTESIAN_POINT('',(1.30000000000002,1.44337567297407,0.));
#12717=CARTESIAN_POINT('',(1.30000000000002,1.44337567297407,0.));
#12718=CARTESIAN_POINT('Origin',(1.30000000000002,0.721687836487031,1.25));
#12719=CARTESIAN_POINT('',(1.30000000000002,0.721687836487031,1.25));
#12720=CARTESIAN_POINT('',(1.30000000000002,0.721687836487031,1.25));
#12721=CARTESIAN_POINT('',(1.30000000000002,0.721687836487031,1.25));
#12722=CARTESIAN_POINT('',(1.30000000000002,0.721687836487031,1.25));
#12723=CARTESIAN_POINT('Origin',(1.30000000000002,-0.721687836487031,1.25));
#12724=CARTESIAN_POINT('',(1.30000000000002,-0.721687836487031,1.25));
#12725=CARTESIAN_POINT('',(1.30000000000002,-0.721687836487031,1.25));
#12726=CARTESIAN_POINT('Origin',(1.30000000000002,-1.44337567297407,0.));
#12727=CARTESIAN_POINT('Origin',(1.30000000000002,-1.44337567297407,0.));
#12728=CARTESIAN_POINT('Origin',(1.30000000000002,-1.44337567297407,0.));
#12729=CARTESIAN_POINT('Origin',(1.30000000000002,-1.44337567297407,0.));
#12730=CARTESIAN_POINT('Origin',(1.30000000000002,-1.44337567297407,0.));
#12731=CARTESIAN_POINT('Origin',(1.30000000000002,-1.44337567297407,0.));
#12732=CARTESIAN_POINT('',(0.,0.,0.));
#12733=CARTESIAN_POINT('Origin',(-997.978312163513,0.,0.));
#12734=CARTESIAN_POINT('',(2.02168783648704,2.16840434497101E-16,0.));
#12735=CARTESIAN_POINT('',(1.3,0.,-1.25));
#12736=CARTESIAN_POINT('',(-997.978312163513,-2.12115047744979E-13,-1732.05080756886));
#12737=CARTESIAN_POINT('',(1.3,-1.08253175473055,-0.625000000000001));
#12738=CARTESIAN_POINT('Origin',(1.3,0.,0.));
#12739=CARTESIAN_POINT('',(1.3,-1.08253175473055,0.625));
#12740=CARTESIAN_POINT('Origin',(1.3,0.,0.));
#12741=CARTESIAN_POINT('',(1.3,1.87789324842145E-16,1.25));
#12742=CARTESIAN_POINT('Origin',(1.3,0.,0.));
#12743=CARTESIAN_POINT('',(1.3,1.08253175473055,0.625000000000001));
#12744=CARTESIAN_POINT('Origin',(1.3,0.,0.));
#12745=CARTESIAN_POINT('',(1.3,1.08253175473055,-0.625));
#12746=CARTESIAN_POINT('Origin',(1.3,0.,0.));
#12747=CARTESIAN_POINT('Origin',(1.3,0.,0.));
#12748=CARTESIAN_POINT('Origin',(2.4,0.,0.));
#12749=CARTESIAN_POINT('',(2.2,-2.69422295812418E-16,-2.2));
#12750=CARTESIAN_POINT('Origin',(2.2,0.,0.));
#12751=CARTESIAN_POINT('',(2.4,-2.44929359829471E-16,-2.));
#12752=CARTESIAN_POINT('Origin',(2.4,-2.69422295812418E-16,-2.2));
#12753=CARTESIAN_POINT('Origin',(2.4,0.,0.));
#12754=CARTESIAN_POINT('Origin',(6.2,0.,0.));
#12755=CARTESIAN_POINT('',(5.81,-2.44929359829471E-16,-2.));
#12756=CARTESIAN_POINT('Origin',(5.81,0.,0.));
#12757=CARTESIAN_POINT('',(6.2,-1.97168134662724E-16,-1.61));
#12758=CARTESIAN_POINT('',(6.2,-1.97168134662724E-16,-1.61));
#12759=CARTESIAN_POINT('Origin',(6.2,0.,0.));
#12760=CARTESIAN_POINT('Origin',(0.,0.,0.));
#12761=CARTESIAN_POINT('',(0.,-2.44929359829471E-16,-2.));
#12762=CARTESIAN_POINT('Origin',(0.,0.,0.));
#12763=CARTESIAN_POINT('',(1.82,-4.65365783675994E-16,-3.8));
#12764=CARTESIAN_POINT('Origin',(1.82,0.,0.));
#12765=CARTESIAN_POINT('',(2.2,-4.65365783675994E-16,-3.8));
#12766=CARTESIAN_POINT('',(0.,-4.65365783675994E-16,-3.8));
#12767=CARTESIAN_POINT('Origin',(2.2,0.,0.));
#12768=CARTESIAN_POINT('Origin',(3.88527472527473,-4.33680868994202E-16,
0.));
#12769=CARTESIAN_POINT('',(4.33680868994202E-16,1.9,0.));
#12770=CARTESIAN_POINT('Origin',(4.33680868994202E-16,0.,0.));
#12771=CARTESIAN_POINT('Origin',(2.16840434497101E-16,0.,0.));
#12772=CARTESIAN_POINT('',(0.,0.721687836487033,1.25));
#12773=CARTESIAN_POINT('',(2.16840434497101E-16,-0.721687836487032,1.25));
#12774=CARTESIAN_POINT('',(0.,-0.721687836487032,1.25));
#12775=CARTESIAN_POINT('',(0.,-1.44337567297406,3.94456587164721E-18));
#12776=CARTESIAN_POINT('',(0.,-1.44337567297406,3.94456587164721E-18));
#12777=CARTESIAN_POINT('',(0.,-0.721687836487032,-1.25));
#12778=CARTESIAN_POINT('',(0.,-0.721687836487032,-1.25));
#12779=CARTESIAN_POINT('',(0.,0.721687836487033,-1.25));
#12780=CARTESIAN_POINT('',(0.,0.721687836487033,-1.25));
#12781=CARTESIAN_POINT('',(0.,1.44337567297407,-1.08420217247849E-16));
#12782=CARTESIAN_POINT('',(0.,1.44337567297407,-1.08420217247849E-16));
#12783=CARTESIAN_POINT('',(0.,0.721687836487033,1.25));
#12784=CARTESIAN_POINT('Origin',(2.2,2.,0.));
#12785=CARTESIAN_POINT('Origin',(6.2,0.,0.));
#12786=CARTESIAN_POINT('Origin',(1.3,-1.44337567297406,3.94456587164721E-18));
#12787=CARTESIAN_POINT('',(1.3,-0.721687836487032,1.25));
#12788=CARTESIAN_POINT('',(1.3,-1.44337567297406,3.94456587164721E-18));
#12789=CARTESIAN_POINT('',(1.3,-1.44337567297406,3.94456587164721E-18));
#12790=CARTESIAN_POINT('',(1.3,-1.44337567297406,3.94456587164721E-18));
#12791=CARTESIAN_POINT('',(1.3,-1.44337567297406,3.94456587164721E-18));
#12792=CARTESIAN_POINT('',(1.3,-0.721687836487032,1.25));
#12793=CARTESIAN_POINT('Origin',(1.3,-0.721687836487032,-1.25));
#12794=CARTESIAN_POINT('',(1.3,-0.721687836487032,-1.25));
#12795=CARTESIAN_POINT('',(1.3,-0.721687836487032,-1.25));
#12796=CARTESIAN_POINT('',(1.3,-0.721687836487032,-1.25));
#12797=CARTESIAN_POINT('',(1.3,-0.721687836487032,-1.25));
#12798=CARTESIAN_POINT('Origin',(1.3,0.721687836487033,-1.25));
#12799=CARTESIAN_POINT('',(1.3,0.721687836487033,-1.25));
#12800=CARTESIAN_POINT('',(1.3,0.721687836487033,-1.25));
#12801=CARTESIAN_POINT('',(1.3,0.721687836487033,-1.25));
#12802=CARTESIAN_POINT('',(1.3,0.721687836487033,-1.25));
#12803=CARTESIAN_POINT('Origin',(1.3,1.44337567297407,-1.08420217247849E-16));
#12804=CARTESIAN_POINT('',(1.3,1.44337567297407,-1.08420217247849E-16));
#12805=CARTESIAN_POINT('',(1.3,1.44337567297407,-1.08420217247849E-16));
#12806=CARTESIAN_POINT('',(1.3,1.44337567297407,-1.08420217247849E-16));
#12807=CARTESIAN_POINT('',(1.3,1.44337567297407,-1.08420217247849E-16));
#12808=CARTESIAN_POINT('Origin',(1.3,0.721687836487033,1.25));
#12809=CARTESIAN_POINT('',(1.3,0.721687836487033,1.25));
#12810=CARTESIAN_POINT('',(1.3,0.721687836487033,1.25));
#12811=CARTESIAN_POINT('',(1.3,0.721687836487033,1.25));
#12812=CARTESIAN_POINT('',(1.3,0.721687836487033,1.25));
#12813=CARTESIAN_POINT('Origin',(1.3,-0.721687836487032,1.25));
#12814=CARTESIAN_POINT('',(1.3,-0.721687836487032,1.25));
#12815=CARTESIAN_POINT('',(1.3,-0.721687836487032,1.25));
#12816=CARTESIAN_POINT('Origin',(1.3,-1.44337567297406,-2.16840434497101E-16));
#12817=CARTESIAN_POINT('Origin',(1.3,-1.44337567297406,-2.16840434497101E-16));
#12818=CARTESIAN_POINT('Origin',(1.3,-1.44337567297406,-2.16840434497101E-16));
#12819=CARTESIAN_POINT('Origin',(1.3,-1.44337567297406,-2.16840434497101E-16));
#12820=CARTESIAN_POINT('Origin',(1.3,-1.44337567297406,-2.16840434497101E-16));
#12821=CARTESIAN_POINT('Origin',(1.3,-1.44337567297406,-2.16840434497101E-16));
#12822=CARTESIAN_POINT('',(0.,0.,0.));
#12823=CARTESIAN_POINT('Origin',(-998.38264973081,0.,0.));
#12824=CARTESIAN_POINT('',(1.61735026918963,2.10855288962746E-17,0.));
#12825=CARTESIAN_POINT('',(1.04,0.,-1.));
#12826=CARTESIAN_POINT('',(-998.38264973081,-2.12115047744979E-13,-1732.05080756886));
#12827=CARTESIAN_POINT('',(1.04,-0.866025403784438,-0.5));
#12828=CARTESIAN_POINT('Origin',(1.04,0.,0.));
#12829=CARTESIAN_POINT('',(1.04,-0.866025403784439,0.5));
#12830=CARTESIAN_POINT('Origin',(1.04,0.,0.));
#12831=CARTESIAN_POINT('',(1.04,-1.87789324842145E-16,1.));
#12832=CARTESIAN_POINT('Origin',(1.04,0.,0.));
#12833=CARTESIAN_POINT('',(1.04,0.866025403784439,0.500000000000001));
#12834=CARTESIAN_POINT('Origin',(1.04,0.,0.));
#12835=CARTESIAN_POINT('',(1.04,0.866025403784439,-0.500000000000001));
#12836=CARTESIAN_POINT('Origin',(1.04,0.,0.));
#12837=CARTESIAN_POINT('Origin',(1.04,0.,0.));
#12838=CARTESIAN_POINT('Origin',(1.75,0.,0.));
#12839=CARTESIAN_POINT('',(1.65,-1.95943487863576E-16,-1.6));
#12840=CARTESIAN_POINT('Origin',(1.65,0.,0.));
#12841=CARTESIAN_POINT('',(1.75,-1.83697019872103E-16,-1.5));
#12842=CARTESIAN_POINT('Origin',(1.75,-1.95943487863576E-16,-1.6));
#12843=CARTESIAN_POINT('Origin',(1.75,0.,0.));
#12844=CARTESIAN_POINT('Origin',(4.65,0.,0.));
#12845=CARTESIAN_POINT('',(4.3695,-1.83697019872103E-16,-1.5));
#12846=CARTESIAN_POINT('Origin',(4.3695,0.,0.));
#12847=CARTESIAN_POINT('',(4.65,-1.4934567715602E-16,-1.2195));
#12848=CARTESIAN_POINT('',(4.65,-1.4934567715602E-16,-1.2195));
#12849=CARTESIAN_POINT('Origin',(4.65,0.,0.));
#12850=CARTESIAN_POINT('Origin',(0.,0.,0.));
#12851=CARTESIAN_POINT('',(0.,-1.83697019872103E-16,-1.5));
#12852=CARTESIAN_POINT('Origin',(0.,0.,0.));
#12853=CARTESIAN_POINT('',(1.27,-3.49024337756996E-16,-2.85));
#12854=CARTESIAN_POINT('Origin',(1.27,0.,0.));
#12855=CARTESIAN_POINT('',(1.65,-3.49024337756996E-16,-2.85));
#12856=CARTESIAN_POINT('',(0.,-3.49024337756996E-16,-2.85));
#12857=CARTESIAN_POINT('Origin',(1.65,0.,0.));
#12858=CARTESIAN_POINT('Origin',(3.03337598425197,-4.33680868994202E-16,
0.));
#12859=CARTESIAN_POINT('',(4.33680868994202E-16,1.425,0.));
#12860=CARTESIAN_POINT('Origin',(4.33680868994202E-16,0.,0.));
#12861=CARTESIAN_POINT('Origin',(2.16840434497101E-16,0.,0.));
#12862=CARTESIAN_POINT('',(0.,0.577350269189626,1.));
#12863=CARTESIAN_POINT('',(2.16840434497101E-16,-0.577350269189626,1.));
#12864=CARTESIAN_POINT('',(0.,-0.577350269189626,1.));
#12865=CARTESIAN_POINT('',(0.,-1.15470053837925,-9.88971598953938E-18));
#12866=CARTESIAN_POINT('',(0.,-1.15470053837925,-9.88971598953938E-18));
#12867=CARTESIAN_POINT('',(0.,-0.577350269189625,-1.));
#12868=CARTESIAN_POINT('',(0.,-0.577350269189625,-1.));
#12869=CARTESIAN_POINT('',(0.,0.577350269189626,-1.));
#12870=CARTESIAN_POINT('',(0.,0.577350269189626,-1.));
#12871=CARTESIAN_POINT('',(0.,1.15470053837925,-1.08420217247849E-16));
#12872=CARTESIAN_POINT('',(0.,1.15470053837925,-1.08420217247849E-16));
#12873=CARTESIAN_POINT('',(0.,0.577350269189626,1.));
#12874=CARTESIAN_POINT('Origin',(1.65,1.5,0.));
#12875=CARTESIAN_POINT('Origin',(4.65,0.,0.));
#12876=CARTESIAN_POINT('Origin',(1.04,-1.15470053837925,-9.88971598953938E-18));
#12877=CARTESIAN_POINT('',(1.04,-0.577350269189626,1.));
#12878=CARTESIAN_POINT('',(1.04,-1.15470053837925,-9.88971598953938E-18));
#12879=CARTESIAN_POINT('',(1.04,-1.15470053837925,-9.88971598953938E-18));
#12880=CARTESIAN_POINT('',(1.04,-1.15470053837925,-9.88971598953938E-18));
#12881=CARTESIAN_POINT('',(1.04,-1.15470053837925,-9.88971598953938E-18));
#12882=CARTESIAN_POINT('',(1.04,-0.577350269189626,1.));
#12883=CARTESIAN_POINT('Origin',(1.04,-0.577350269189625,-1.));
#12884=CARTESIAN_POINT('',(1.04,-0.577350269189625,-1.));
#12885=CARTESIAN_POINT('',(1.04,-0.577350269189625,-1.));
#12886=CARTESIAN_POINT('',(1.04,-0.577350269189625,-1.));
#12887=CARTESIAN_POINT('',(1.04,-0.577350269189625,-1.));
#12888=CARTESIAN_POINT('Origin',(1.04,0.577350269189626,-1.));
#12889=CARTESIAN_POINT('',(1.04,0.577350269189626,-1.));
#12890=CARTESIAN_POINT('',(1.04,0.577350269189626,-1.));
#12891=CARTESIAN_POINT('',(1.04,0.577350269189626,-1.));
#12892=CARTESIAN_POINT('',(1.04,0.577350269189626,-1.));
#12893=CARTESIAN_POINT('Origin',(1.04,1.15470053837925,-1.08420217247849E-16));
#12894=CARTESIAN_POINT('',(1.04,1.15470053837925,-1.08420217247849E-16));
#12895=CARTESIAN_POINT('',(1.04,1.15470053837925,-1.08420217247849E-16));
#12896=CARTESIAN_POINT('',(1.04,1.15470053837925,-1.08420217247849E-16));
#12897=CARTESIAN_POINT('',(1.04,1.15470053837925,-1.08420217247849E-16));
#12898=CARTESIAN_POINT('Origin',(1.04,0.577350269189626,1.));
#12899=CARTESIAN_POINT('',(1.04,0.577350269189626,1.));
#12900=CARTESIAN_POINT('',(1.04,0.577350269189626,1.));
#12901=CARTESIAN_POINT('',(1.04,0.577350269189626,1.));
#12902=CARTESIAN_POINT('',(1.04,0.577350269189626,1.));
#12903=CARTESIAN_POINT('Origin',(1.04,-0.577350269189626,1.));
#12904=CARTESIAN_POINT('',(1.04,-0.577350269189626,1.));
#12905=CARTESIAN_POINT('',(1.04,-0.577350269189626,1.));
#12906=CARTESIAN_POINT('Origin',(1.04,-1.15470053837925,0.));
#12907=CARTESIAN_POINT('Origin',(1.04,-1.15470053837925,0.));
#12908=CARTESIAN_POINT('Origin',(1.04,-1.15470053837925,0.));
#12909=CARTESIAN_POINT('Origin',(1.04,-1.15470053837925,0.));
#12910=CARTESIAN_POINT('Origin',(1.04,-1.15470053837925,0.));
#12911=CARTESIAN_POINT('Origin',(1.04,-1.15470053837925,0.));
#12912=CARTESIAN_POINT('',(0.,0.,0.));
#12913=CARTESIAN_POINT('',(41.9999999999996,7.49999999999993,18.0000000000011));
#12914=CARTESIAN_POINT('',(24.2509101232364,3.99999999999996,-35.6059594611192));
#12915=CARTESIAN_POINT('',(6.50182024647033,7.,53.2119189222396));
#12916=CARTESIAN_POINT('',(12.,24.2,-12.5));
#12917=CARTESIAN_POINT('',(-23.0666260508084,20.2,48.1417134466452));
#12918=CARTESIAN_POINT('',(12.,-2.2,12.5));
#12919=CARTESIAN_POINT('',(72.,-1.65,-30.));
#12920=CARTESIAN_POINT('',(6.50182024647227,15.,-53.2119189222384));
#12921=CARTESIAN_POINT('',(24.250910123236,4.,35.6059594611202));
#12922=CARTESIAN_POINT('',(24.250910123236,15.,-35.6059594611202));
#12923=CARTESIAN_POINT('',(-5.53331302540547,15.,30.3208567233224));
#12924=CARTESIAN_POINT('',(41.9999999999996,7.49999999999967,-18.0000000000011));
#12925=CARTESIAN_POINT('',(-5.53331302540554,4.,30.3208567233224));
#12926=CARTESIAN_POINT('',(24.2509101232359,15.,35.6059594611203));
#12927=CARTESIAN_POINT('',(-5.53331302540509,15.,-30.3208567233221));
#12928=CARTESIAN_POINT('',(-5.53331302540507,3.99999999999996,-30.3208567233221));
#12929=CARTESIAN_POINT('',(12.,24.2,12.5));
#12930=CARTESIAN_POINT('',(42.,24.2,-18.));
#12931=CARTESIAN_POINT('',(42.,24.2,18.));
#12932=CARTESIAN_POINT('',(6.50182024647378,20.2,53.2119189222391));
#12933=CARTESIAN_POINT('',(-23.0666260508092,20.2,-48.1417134466444));
#12934=CARTESIAN_POINT('',(6.50182024647298,20.2,-53.2119189222383));
#12935=CARTESIAN_POINT('',(12.,-2.2,-12.5));
#12936=CARTESIAN_POINT('',(42.,-2.2,18.));
#12937=CARTESIAN_POINT('',(42.,-2.2,-18.));
#12938=CARTESIAN_POINT('',(-23.0666260508084,1.8,48.1417134466452));
#12939=CARTESIAN_POINT('',(6.50182024647378,1.8,53.2119189222391));
#12940=CARTESIAN_POINT('',(-23.0666260508092,1.79999999999996,-48.1417134466444));
#12941=CARTESIAN_POINT('',(6.50182024647298,1.79999999999996,-53.2119189222383));
#12942=CARTESIAN_POINT('',(72.,-1.65,30.));
#12943=CARTESIAN_POINT('',(7.,-1.65,0.));
#12944=CARTESIAN_POINT('',(72.,23.65,-30.));
#12945=CARTESIAN_POINT('',(72.,23.65,30.));
#12946=CARTESIAN_POINT('',(7.00000000000001,23.65,0.));
#12947=UNCERTAINTY_MEASURE_WITH_UNIT(LENGTH_MEASURE(0.01),#12967,
'DISTANCE_ACCURACY_VALUE',
'Maximum model space distance between geometric entities at asserted c
onnectivities');
#12948=UNCERTAINTY_MEASURE_WITH_UNIT(LENGTH_MEASURE(0.01),#12967,
'DISTANCE_ACCURACY_VALUE',
'Maximum model space distance between geometric entities at asserted c
onnectivities');
#12949=UNCERTAINTY_MEASURE_WITH_UNIT(LENGTH_MEASURE(0.01),#12967,
'DISTANCE_ACCURACY_VALUE',
'Maximum model space distance between geometric entities at asserted c
onnectivities');
#12950=UNCERTAINTY_MEASURE_WITH_UNIT(LENGTH_MEASURE(0.01),#12967,
'DISTANCE_ACCURACY_VALUE',
'Maximum model space distance between geometric entities at asserted c
onnectivities');
#12951=UNCERTAINTY_MEASURE_WITH_UNIT(LENGTH_MEASURE(0.01),#12967,
'DISTANCE_ACCURACY_VALUE',
'Maximum model space distance between geometric entities at asserted c
onnectivities');
#12952=UNCERTAINTY_MEASURE_WITH_UNIT(LENGTH_MEASURE(0.01),#12967,
'DISTANCE_ACCURACY_VALUE',
'Maximum model space distance between geometric entities at asserted c
onnectivities');
#12953=UNCERTAINTY_MEASURE_WITH_UNIT(LENGTH_MEASURE(0.01),#12967,
'DISTANCE_ACCURACY_VALUE',
'Maximum model space distance between geometric entities at asserted c
onnectivities');
#12954=UNCERTAINTY_MEASURE_WITH_UNIT(LENGTH_MEASURE(0.01),#12967,
'DISTANCE_ACCURACY_VALUE',
'Maximum model space distance between geometric entities at asserted c
onnectivities');
#12955=UNCERTAINTY_MEASURE_WITH_UNIT(LENGTH_MEASURE(0.01),#12967,
'DISTANCE_ACCURACY_VALUE',
'Maximum model space distance between geometric entities at asserted c
onnectivities');
#12956=UNCERTAINTY_MEASURE_WITH_UNIT(LENGTH_MEASURE(0.01),#12967,
'DISTANCE_ACCURACY_VALUE',
'Maximum model space distance between geometric entities at asserted c
onnectivities');
#12957=(
GEOMETRIC_REPRESENTATION_CONTEXT(3)
GLOBAL_UNCERTAINTY_ASSIGNED_CONTEXT((#12947))
GLOBAL_UNIT_ASSIGNED_CONTEXT((#12967,#12969,#12970))
REPRESENTATION_CONTEXT('','3D')
);
#12958=(
GEOMETRIC_REPRESENTATION_CONTEXT(3)
GLOBAL_UNCERTAINTY_ASSIGNED_CONTEXT((#12948))
GLOBAL_UNIT_ASSIGNED_CONTEXT((#12967,#12969,#12970))
REPRESENTATION_CONTEXT('','3D')
);
#12959=(
GEOMETRIC_REPRESENTATION_CONTEXT(3)
GLOBAL_UNCERTAINTY_ASSIGNED_CONTEXT((#12949))
GLOBAL_UNIT_ASSIGNED_CONTEXT((#12967,#12969,#12970))
REPRESENTATION_CONTEXT('','3D')
);
#12960=(
GEOMETRIC_REPRESENTATION_CONTEXT(3)
GLOBAL_UNCERTAINTY_ASSIGNED_CONTEXT((#12950))
GLOBAL_UNIT_ASSIGNED_CONTEXT((#12967,#12969,#12970))
REPRESENTATION_CONTEXT('','3D')
);
#12961=(
GEOMETRIC_REPRESENTATION_CONTEXT(3)
GLOBAL_UNCERTAINTY_ASSIGNED_CONTEXT((#12951))
GLOBAL_UNIT_ASSIGNED_CONTEXT((#12967,#12969,#12970))
REPRESENTATION_CONTEXT('','3D')
);
#12962=(
GEOMETRIC_REPRESENTATION_CONTEXT(3)
GLOBAL_UNCERTAINTY_ASSIGNED_CONTEXT((#12952))
GLOBAL_UNIT_ASSIGNED_CONTEXT((#12967,#12969,#12970))
REPRESENTATION_CONTEXT('','3D')
);
#12963=(
GEOMETRIC_REPRESENTATION_CONTEXT(3)
GLOBAL_UNCERTAINTY_ASSIGNED_CONTEXT((#12953))
GLOBAL_UNIT_ASSIGNED_CONTEXT((#12967,#12969,#12970))
REPRESENTATION_CONTEXT('','3D')
);
#12964=(
GEOMETRIC_REPRESENTATION_CONTEXT(3)
GLOBAL_UNCERTAINTY_ASSIGNED_CONTEXT((#12954))
GLOBAL_UNIT_ASSIGNED_CONTEXT((#12967,#12969,#12970))
REPRESENTATION_CONTEXT('','3D')
);
#12965=(
GEOMETRIC_REPRESENTATION_CONTEXT(3)
GLOBAL_UNCERTAINTY_ASSIGNED_CONTEXT((#12955))
GLOBAL_UNIT_ASSIGNED_CONTEXT((#12967,#12969,#12970))
REPRESENTATION_CONTEXT('','3D')
);
#12966=(
GEOMETRIC_REPRESENTATION_CONTEXT(3)
GLOBAL_UNCERTAINTY_ASSIGNED_CONTEXT((#12956))
GLOBAL_UNIT_ASSIGNED_CONTEXT((#12967,#12969,#12970))
REPRESENTATION_CONTEXT('','3D')
);
#12967=(
LENGTH_UNIT()
NAMED_UNIT(*)
SI_UNIT(.MILLI.,.METRE.)
);
#12968=(
LENGTH_UNIT()
NAMED_UNIT(*)
SI_UNIT($,.METRE.)
);
#12969=(
NAMED_UNIT(*)
PLANE_ANGLE_UNIT()
SI_UNIT($,.RADIAN.)
);
#12970=(
NAMED_UNIT(*)
SI_UNIT($,.STERADIAN.)
SOLID_ANGLE_UNIT()
);
#12971=SHAPE_DEFINITION_REPRESENTATION(#12980,#13024);
#12972=SHAPE_DEFINITION_REPRESENTATION(#12981,#13025);
#12973=SHAPE_DEFINITION_REPRESENTATION(#12982,#13026);
#12974=SHAPE_DEFINITION_REPRESENTATION(#12983,#13027);
#12975=SHAPE_DEFINITION_REPRESENTATION(#12984,#13028);
#12976=SHAPE_DEFINITION_REPRESENTATION(#12985,#13029);
#12977=SHAPE_DEFINITION_REPRESENTATION(#12986,#13030);
#12978=SHAPE_DEFINITION_REPRESENTATION(#12987,#13031);
#12979=SHAPE_DEFINITION_REPRESENTATION(#12988,#13032);
#12980=PRODUCT_DEFINITION_SHAPE('',$,#13034);
#12981=PRODUCT_DEFINITION_SHAPE('',$,#13035);
#12982=PRODUCT_DEFINITION_SHAPE('',$,#13036);
#12983=PRODUCT_DEFINITION_SHAPE('',$,#13037);
#12984=PRODUCT_DEFINITION_SHAPE('',$,#13038);
#12985=PRODUCT_DEFINITION_SHAPE('',$,#13039);
#12986=PRODUCT_DEFINITION_SHAPE('',$,#13040);
#12987=PRODUCT_DEFINITION_SHAPE('',$,#13041);
#12988=PRODUCT_DEFINITION_SHAPE('',$,#13042);
#12989=PRODUCT_DEFINITION_SHAPE($,$,#116);
#12990=PRODUCT_DEFINITION_SHAPE($,$,#117);
#12991=PRODUCT_DEFINITION_SHAPE($,$,#118);
#12992=PRODUCT_DEFINITION_SHAPE($,$,#119);
#12993=PRODUCT_DEFINITION_SHAPE($,$,#120);
#12994=PRODUCT_DEFINITION_SHAPE($,$,#121);
#12995=PRODUCT_DEFINITION_SHAPE($,$,#122);
#12996=PRODUCT_DEFINITION_SHAPE($,$,#123);
#12997=PRODUCT_DEFINITION_SHAPE($,$,#124);
#12998=PRODUCT_DEFINITION_SHAPE($,$,#125);
#12999=PRODUCT_DEFINITION_SHAPE($,$,#126);
#13000=PRODUCT_DEFINITION_SHAPE($,$,#127);
#13001=PRODUCT_DEFINITION_SHAPE($,$,#128);
#13002=PRODUCT_DEFINITION_SHAPE($,$,#129);
#13003=PRODUCT_DEFINITION_SHAPE($,$,#130);
#13004=PRODUCT_DEFINITION_SHAPE($,$,#131);
#13005=PRODUCT_DEFINITION_SHAPE($,$,#132);
#13006=PRODUCT_DEFINITION_SHAPE($,$,#133);
#13007=PRODUCT_DEFINITION_SHAPE($,$,#134);
#13008=PRODUCT_DEFINITION_SHAPE($,$,#135);
#13009=PRODUCT_DEFINITION_SHAPE($,$,#136);
#13010=PRODUCT_DEFINITION_SHAPE($,$,#137);
#13011=PRODUCT_DEFINITION_SHAPE($,$,#138);
#13012=PRODUCT_DEFINITION_SHAPE($,$,#139);
#13013=PRODUCT_DEFINITION_SHAPE($,$,#140);
#13014=PRODUCT_DEFINITION_SHAPE($,$,#141);
#13015=PRODUCT_DEFINITION_SHAPE($,$,#142);
#13016=PRODUCT_DEFINITION_SHAPE($,$,#143);
#13017=PRODUCT_DEFINITION_SHAPE($,$,#144);
#13018=PRODUCT_DEFINITION_SHAPE($,$,#145);
#13019=PRODUCT_DEFINITION_SHAPE($,$,#146);
#13020=PRODUCT_DEFINITION_SHAPE($,$,#147);
#13021=PRODUCT_DEFINITION_SHAPE($,$,#148);
#13022=PRODUCT_DEFINITION_SHAPE($,$,#149);
#13023=PRODUCT_DEFINITION_SHAPE($,$,#150);
#13024=SHAPE_REPRESENTATION('',(#5679,#6187,#6188,#6189,#6190,#6191,#6192,
#6193,#6194,#6195,#6196,#6197,#6198,#6199,#6200,#6201,#6202,#6203,#6204,
#6205,#6206,#6207,#6208,#6209,#6210,#6211,#6212,#6213,#6214,#6215,#6216,
#6217,#6218,#6219,#6220,#6221),#12957);
#13025=SHAPE_REPRESENTATION('',(#5680),#12958);
#13026=SHAPE_REPRESENTATION('',(#5783),#12959);
#13027=SHAPE_REPRESENTATION('',(#5884),#12960);
#13028=SHAPE_REPRESENTATION('',(#6026),#12961);
#13029=SHAPE_REPRESENTATION('',(#6043),#12962);
#13030=SHAPE_REPRESENTATION('',(#6079),#12963);
#13031=SHAPE_REPRESENTATION('',(#6115),#12964);
#13032=SHAPE_REPRESENTATION('',(#6151),#12965);
#13033=PRODUCT_DEFINITION_CONTEXT('part definition',#13062,'design');
#13034=PRODUCT_DEFINITION('MAT-042','(Unsaved)',#13043,#13033);
#13035=PRODUCT_DEFINITION('Base Frame','Base Frame',#13044,#13033);
#13036=PRODUCT_DEFINITION('Cam Grip','Cam Grip',#13045,#13033);
#13037=PRODUCT_DEFINITION('Gear','Gear',#13046,#13033);
#13038=PRODUCT_DEFINITION('Link','Link',#13047,#13033);
#13039=PRODUCT_DEFINITION('Button Head Cap Screw M4x0.7x20',
'Button Head Cap Screw M4x0.7x20',#13048,#13033);
#13040=PRODUCT_DEFINITION('Button Head Cap Screw M4x0.7x8',
'Button Head Cap Screw M4x0.7x8',#13049,#13033);
#13041=PRODUCT_DEFINITION('Button Head Cap Screw M4x0.7x4',
'Button Head Cap Screw M4x0.7x4',#13050,#13033);
#13042=PRODUCT_DEFINITION('Button Head Cap Screw M3x0.5x3',
'Button Head Cap Screw M3x0.5x3',#13051,#13033);
#13043=PRODUCT_DEFINITION_FORMATION('',$,#13064);
#13044=PRODUCT_DEFINITION_FORMATION('',$,#13065);
#13045=PRODUCT_DEFINITION_FORMATION('',$,#13066);
#13046=PRODUCT_DEFINITION_FORMATION('',$,#13067);
#13047=PRODUCT_DEFINITION_FORMATION('',$,#13068);
#13048=PRODUCT_DEFINITION_FORMATION('',$,#13069);
#13049=PRODUCT_DEFINITION_FORMATION('',$,#13070);
#13050=PRODUCT_DEFINITION_FORMATION('',$,#13071);
#13051=PRODUCT_DEFINITION_FORMATION('',$,#13072);
#13052=PRODUCT_RELATED_PRODUCT_CATEGORY('(Unsaved)','(Unsaved)',(#13064));
#13053=PRODUCT_RELATED_PRODUCT_CATEGORY('Base Frame','Base Frame',(#13065));
#13054=PRODUCT_RELATED_PRODUCT_CATEGORY('Cam Grip','Cam Grip',(#13066));
#13055=PRODUCT_RELATED_PRODUCT_CATEGORY('Gear','Gear',(#13067));
#13056=PRODUCT_RELATED_PRODUCT_CATEGORY('Link','Link',(#13068));
#13057=PRODUCT_RELATED_PRODUCT_CATEGORY(
'Button Head Cap Screw M4x0.7x20','Button Head Cap Screw M4x0.7x20',(#13069));
#13058=PRODUCT_RELATED_PRODUCT_CATEGORY(
'Button Head Cap Screw M4x0.7x8','Button Head Cap Screw M4x0.7x8',(#13070));
#13059=PRODUCT_RELATED_PRODUCT_CATEGORY(
'Button Head Cap Screw M4x0.7x4','Button Head Cap Screw M4x0.7x4',(#13071));
#13060=PRODUCT_RELATED_PRODUCT_CATEGORY(
'Button Head Cap Screw M3x0.5x3','Button Head Cap Screw M3x0.5x3',(#13072));
#13061=APPLICATION_PROTOCOL_DEFINITION('international standard',
'automotive_design',2009,#13062);
#13062=APPLICATION_CONTEXT(
'Core Data for Automotive Mechanical Design Process');
#13063=PRODUCT_CONTEXT('part definition',#13062,'mechanical');
#13064=PRODUCT('MAT-042','(Unsaved)','STEP AP214',(#13063));
#13065=PRODUCT('Base Frame','Base Frame',$,(#13063));
#13066=PRODUCT('Cam Grip','Cam Grip',$,(#13063));
#13067=PRODUCT('Gear','Gear',$,(#13063));
#13068=PRODUCT('Link','Link',$,(#13063));
#13069=PRODUCT('Button Head Cap Screw M4x0.7x20',
'Button Head Cap Screw M4x0.7x20',$,(#13063));
#13070=PRODUCT('Button Head Cap Screw M4x0.7x8',
'Button Head Cap Screw M4x0.7x8',$,(#13063));
#13071=PRODUCT('Button Head Cap Screw M4x0.7x4',
'Button Head Cap Screw M4x0.7x4',$,(#13063));
#13072=PRODUCT('Button Head Cap Screw M3x0.5x3',
'Button Head Cap Screw M3x0.5x3',$,(#13063));
#13073=PRESENTATION_STYLE_ASSIGNMENT((#13078));
#13074=PRESENTATION_STYLE_ASSIGNMENT((#13079));
#13075=PRESENTATION_STYLE_ASSIGNMENT((#13080));
#13076=PRESENTATION_STYLE_ASSIGNMENT((#13081));
#13077=PRESENTATION_STYLE_ASSIGNMENT((#13082));
#13078=SURFACE_STYLE_USAGE(.BOTH.,#13083);
#13079=SURFACE_STYLE_USAGE(.BOTH.,#13084);
#13080=SURFACE_STYLE_USAGE(.BOTH.,#13085);
#13081=SURFACE_STYLE_USAGE(.BOTH.,#13086);
#13082=SURFACE_STYLE_USAGE(.BOTH.,#13087);
#13083=SURFACE_SIDE_STYLE('',(#13088));
#13084=SURFACE_SIDE_STYLE('',(#13089));
#13085=SURFACE_SIDE_STYLE('',(#13090));
#13086=SURFACE_SIDE_STYLE('',(#13091));
#13087=SURFACE_SIDE_STYLE('',(#13092));
#13088=SURFACE_STYLE_FILL_AREA(#13093);
#13089=SURFACE_STYLE_FILL_AREA(#13094);
#13090=SURFACE_STYLE_FILL_AREA(#13095);
#13091=SURFACE_STYLE_FILL_AREA(#13096);
#13092=SURFACE_STYLE_FILL_AREA(#13097);
#13093=FILL_AREA_STYLE('Steel - Satin',(#13098));
#13094=FILL_AREA_STYLE('Opaque(20,51,87)',(#13099));
#13095=FILL_AREA_STYLE('Opaque(31,36,43)',(#13100));
#13096=FILL_AREA_STYLE('Opaque(227,224,212)',(#13101));
#13097=FILL_AREA_STYLE('Opaque(61,176,222)',(#13102));
#13098=FILL_AREA_STYLE_COLOUR('Steel - Satin',#13103);
#13099=FILL_AREA_STYLE_COLOUR('Opaque(20,51,87)',#13104);
#13100=FILL_AREA_STYLE_COLOUR('Opaque(31,36,43)',#13105);
#13101=FILL_AREA_STYLE_COLOUR('Opaque(227,224,212)',#13106);
#13102=FILL_AREA_STYLE_COLOUR('Opaque(61,176,222)',#13107);
#13103=COLOUR_RGB('Steel - Satin',0.627450980392157,0.627450980392157,0.627450980392157);
#13104=COLOUR_RGB('Opaque(20,51,87)',0.0784313725490196,0.2,0.341176470588235);
#13105=COLOUR_RGB('Opaque(31,36,43)',0.12156862745098,0.141176470588235,
0.168627450980392);
#13106=COLOUR_RGB('Opaque(227,224,212)',0.890196078431372,0.87843137254902,
0.831372549019608);
#13107=COLOUR_RGB('Opaque(61,176,222)',0.23921568627451,0.690196078431373,
0.870588235294118);
ENDSEC;
END-ISO-10303-21;
